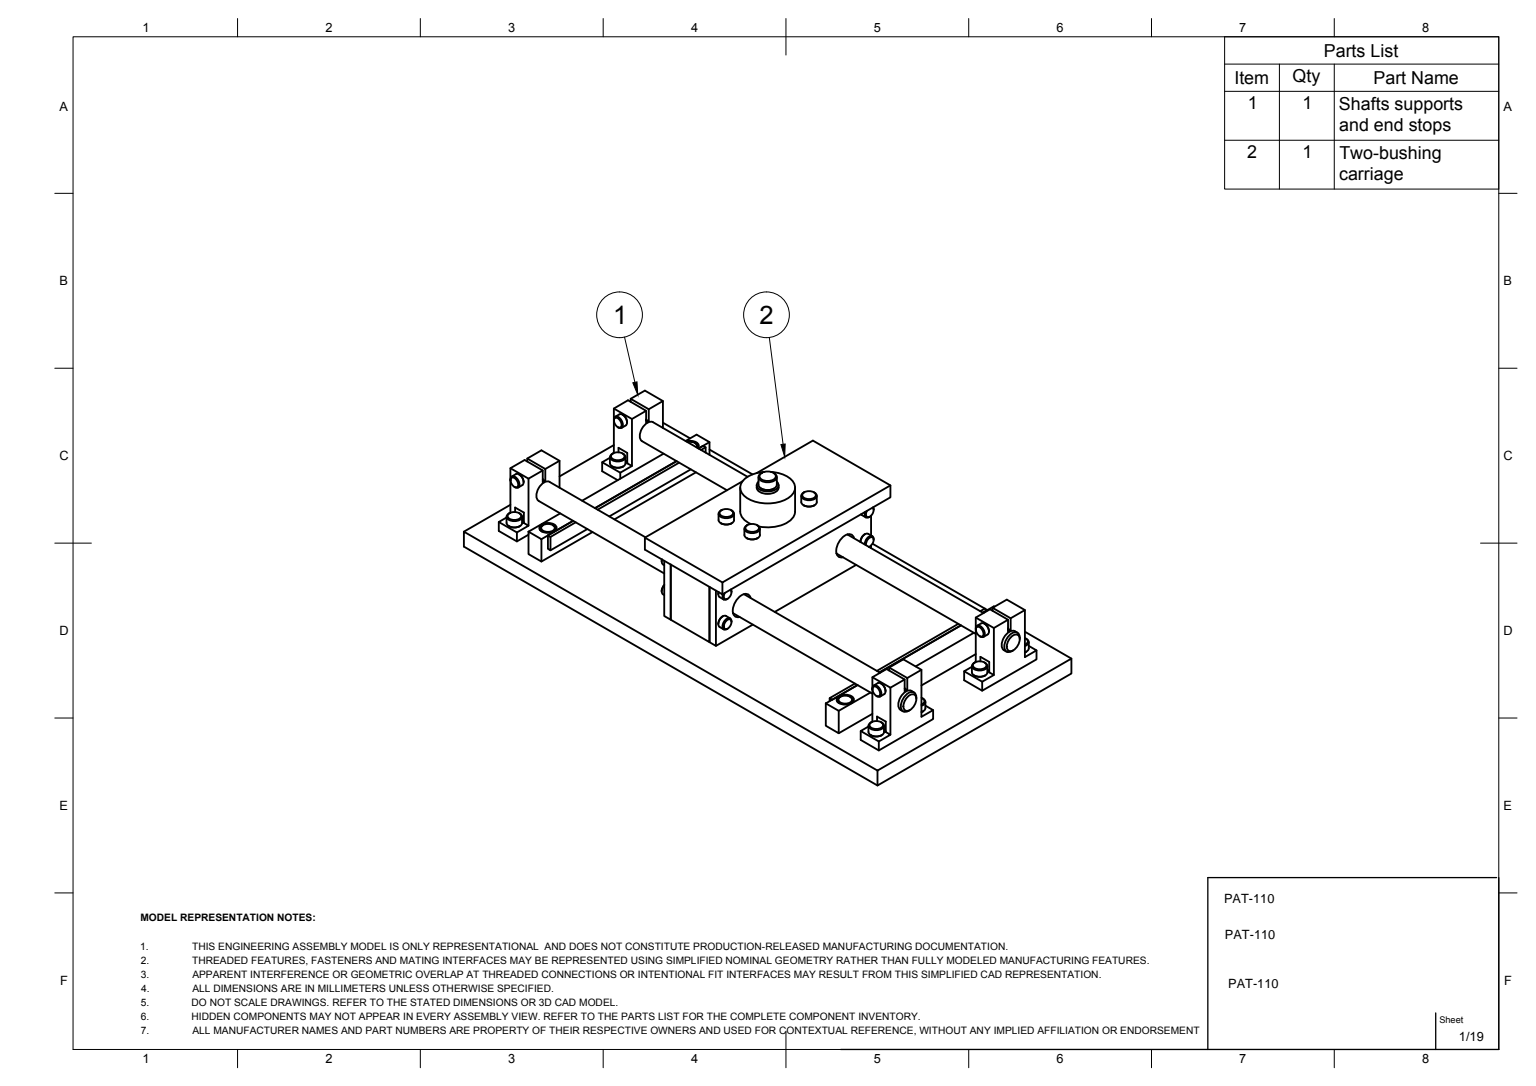
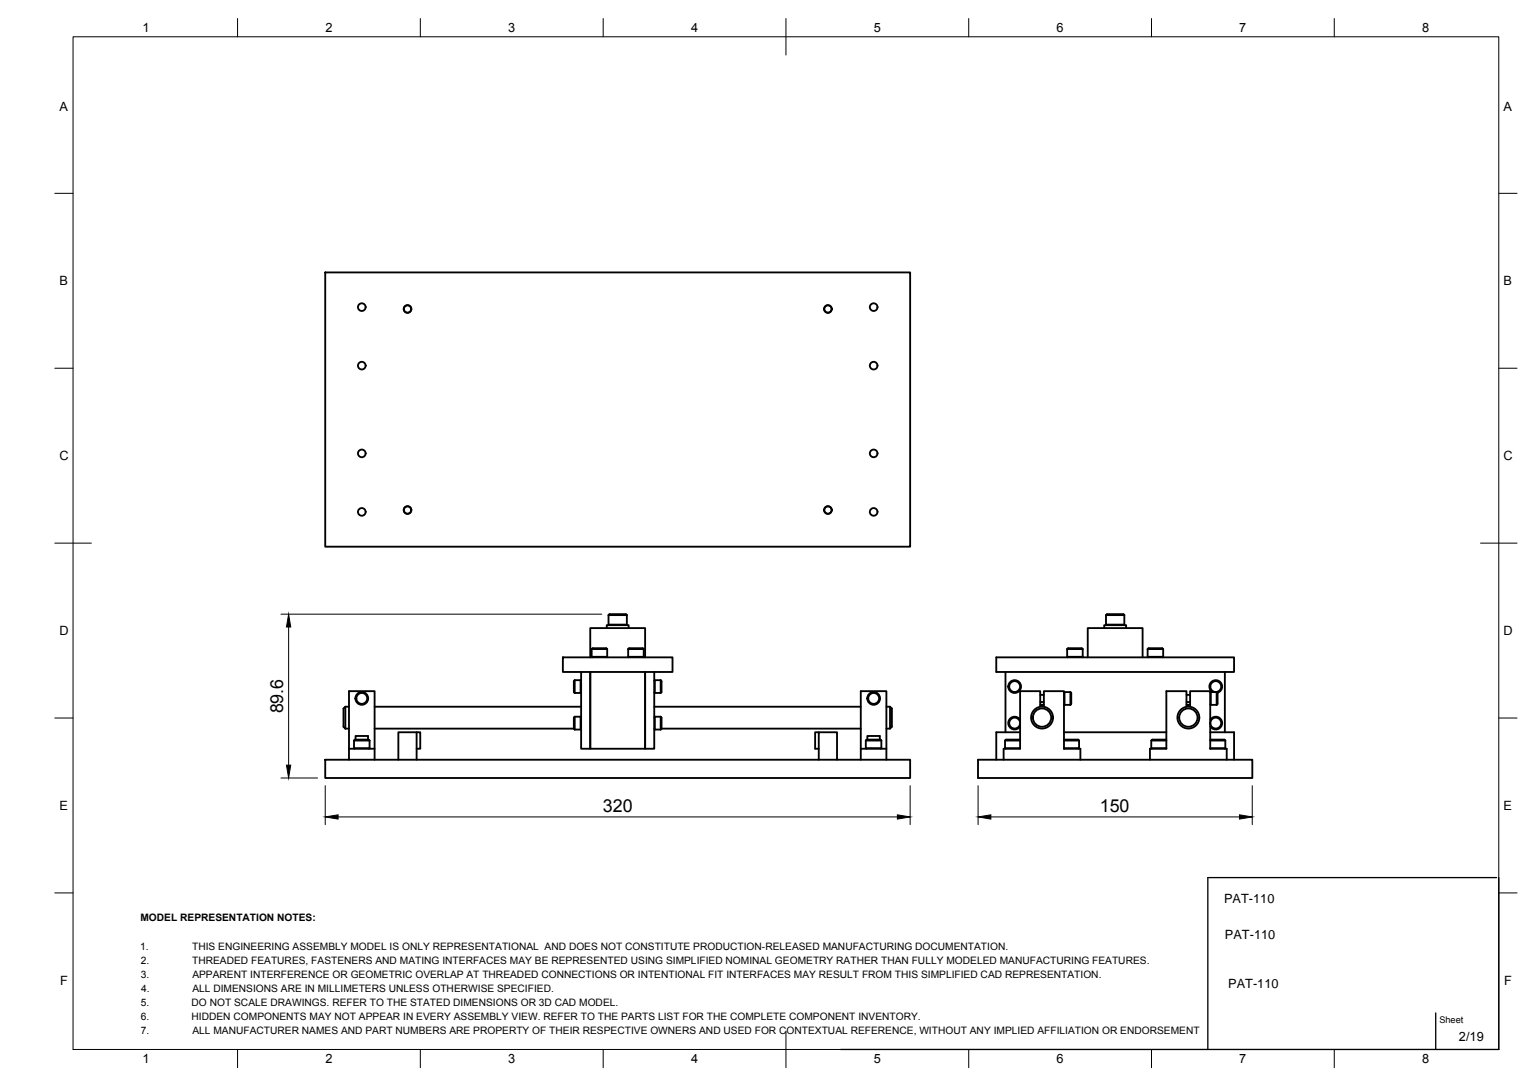
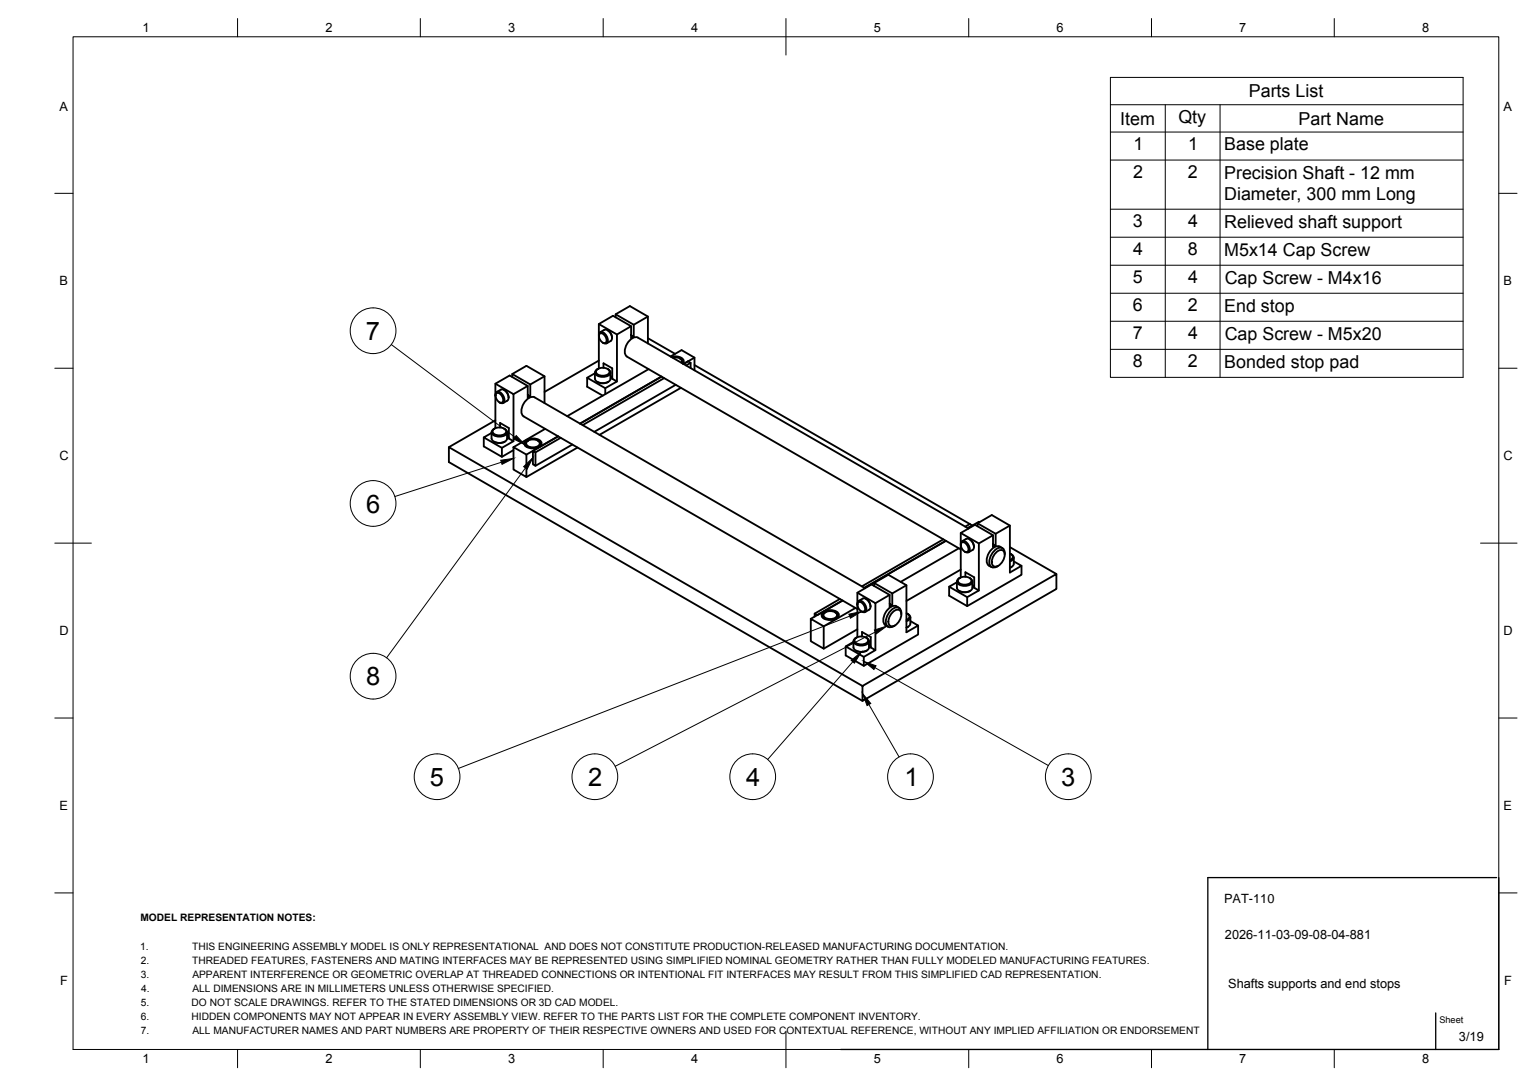
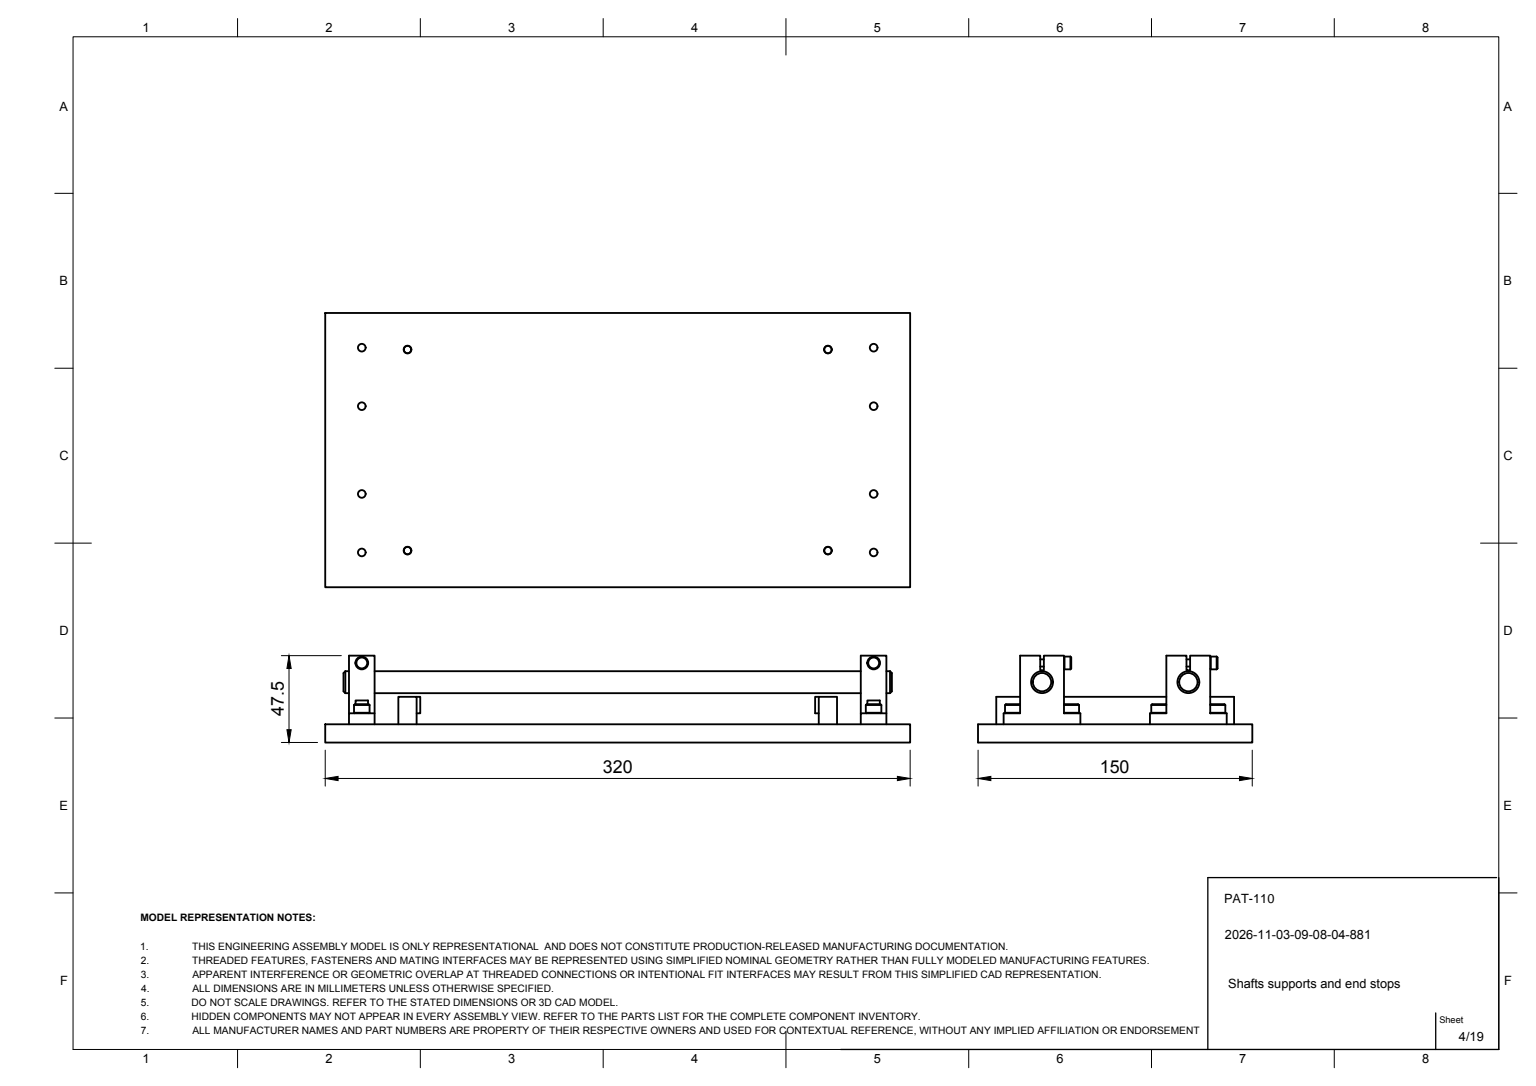
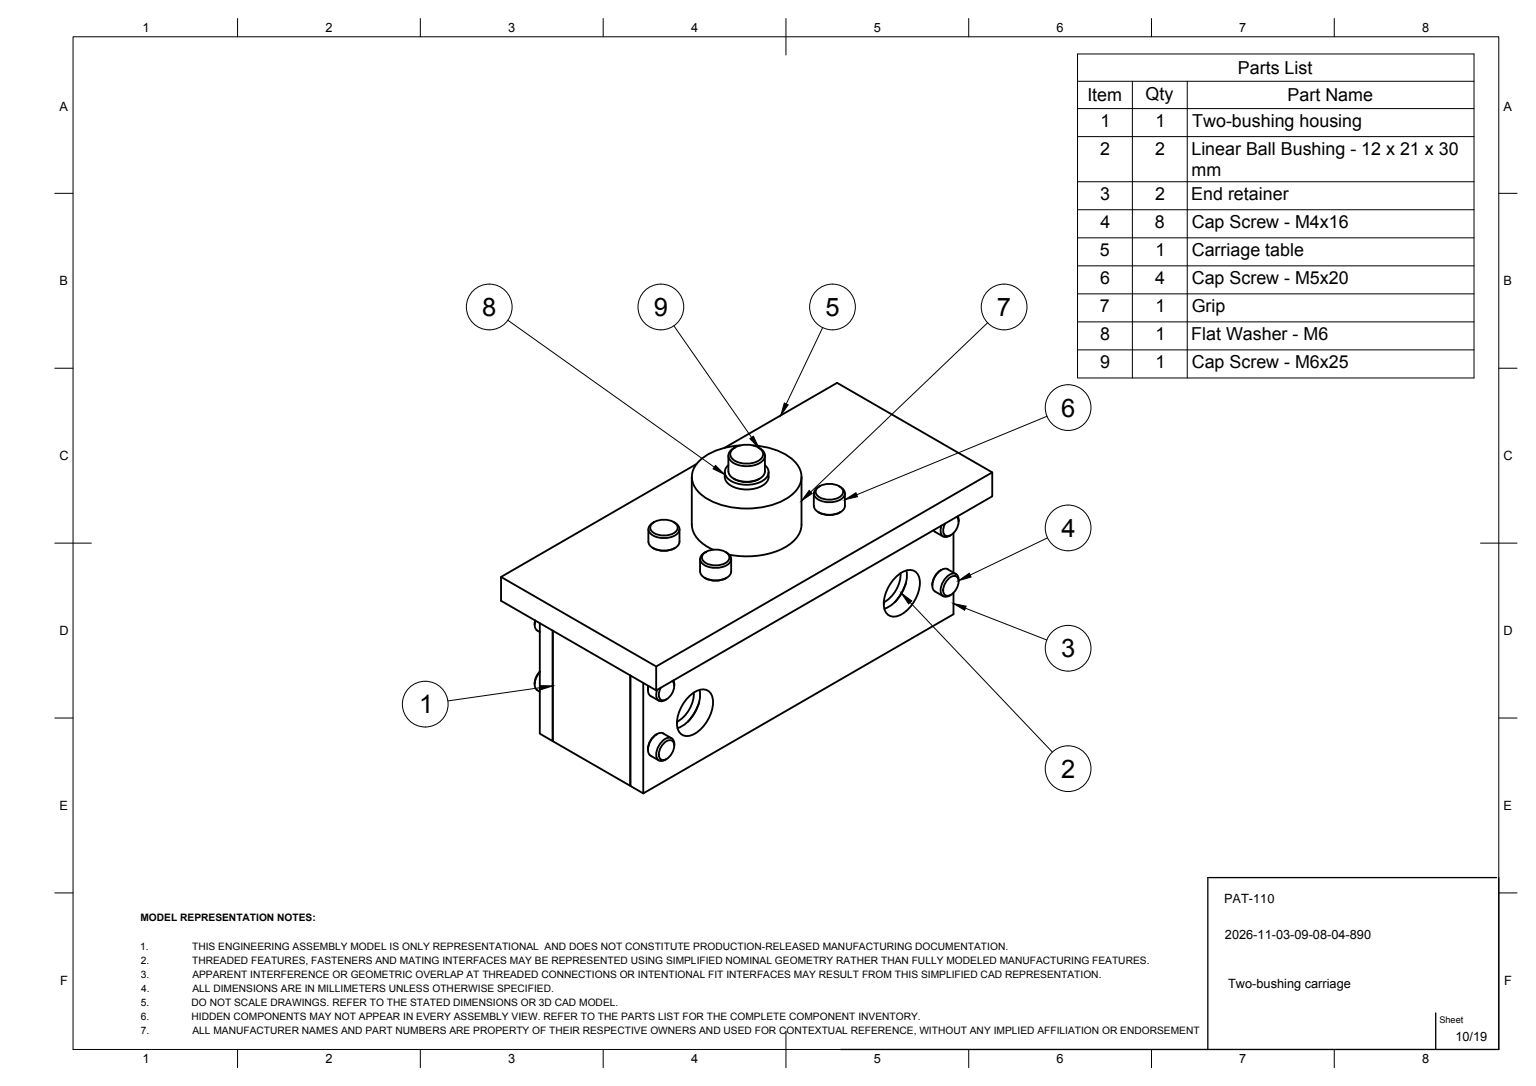
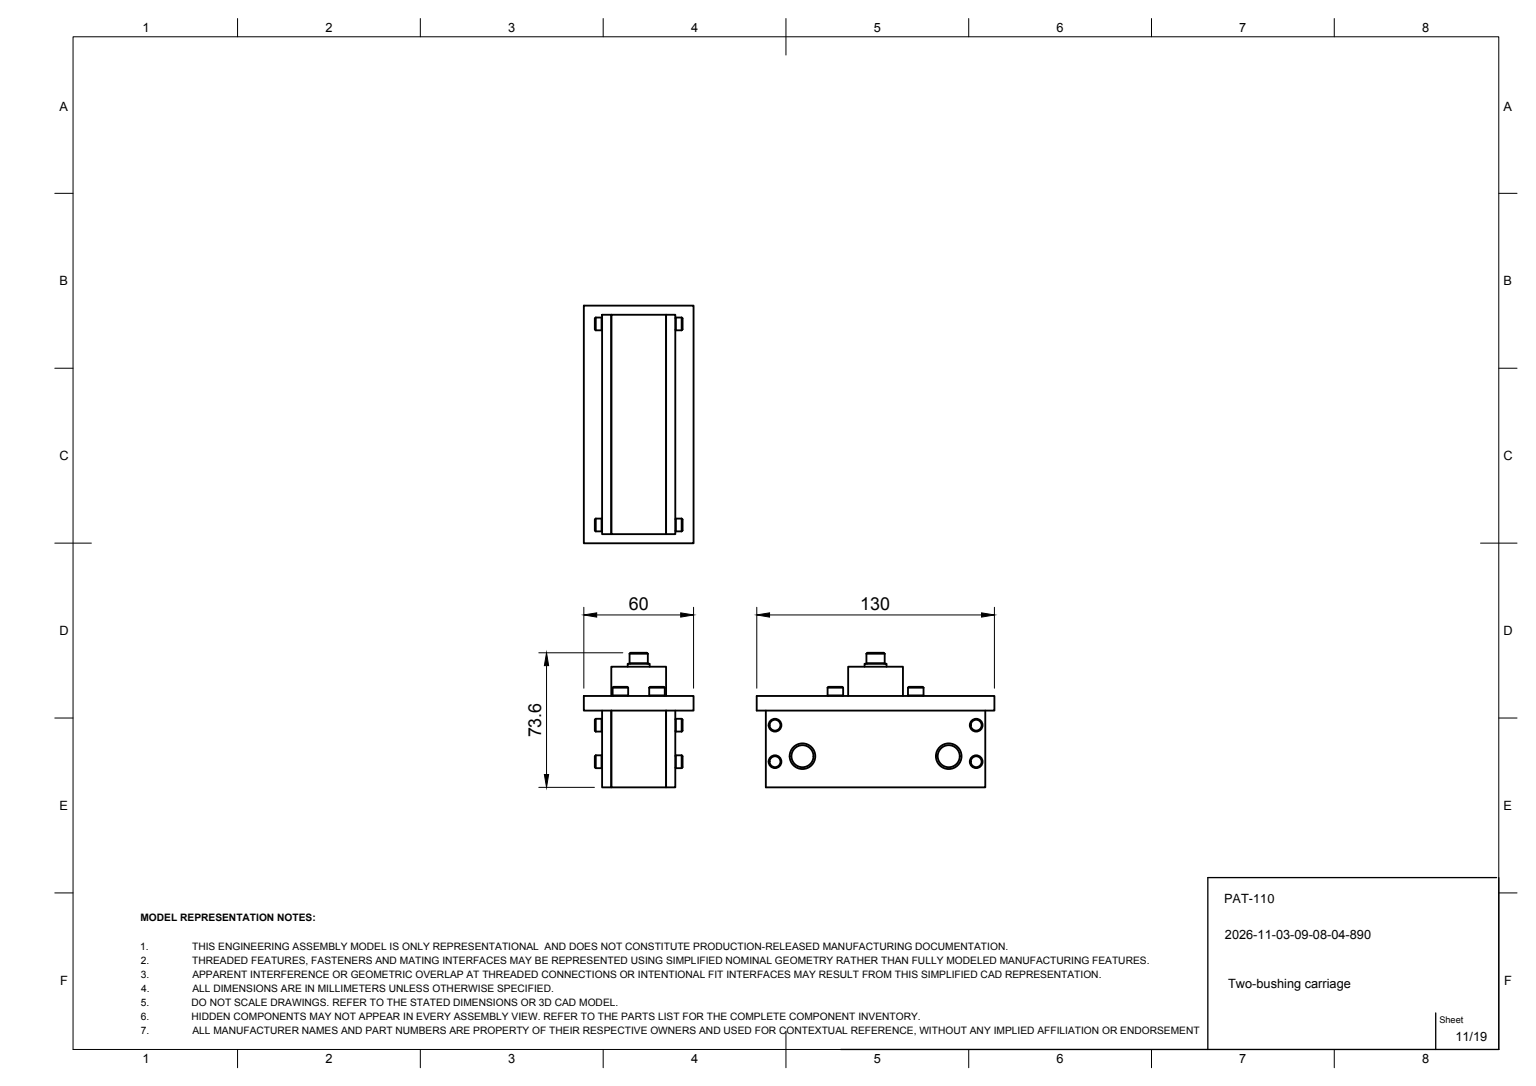
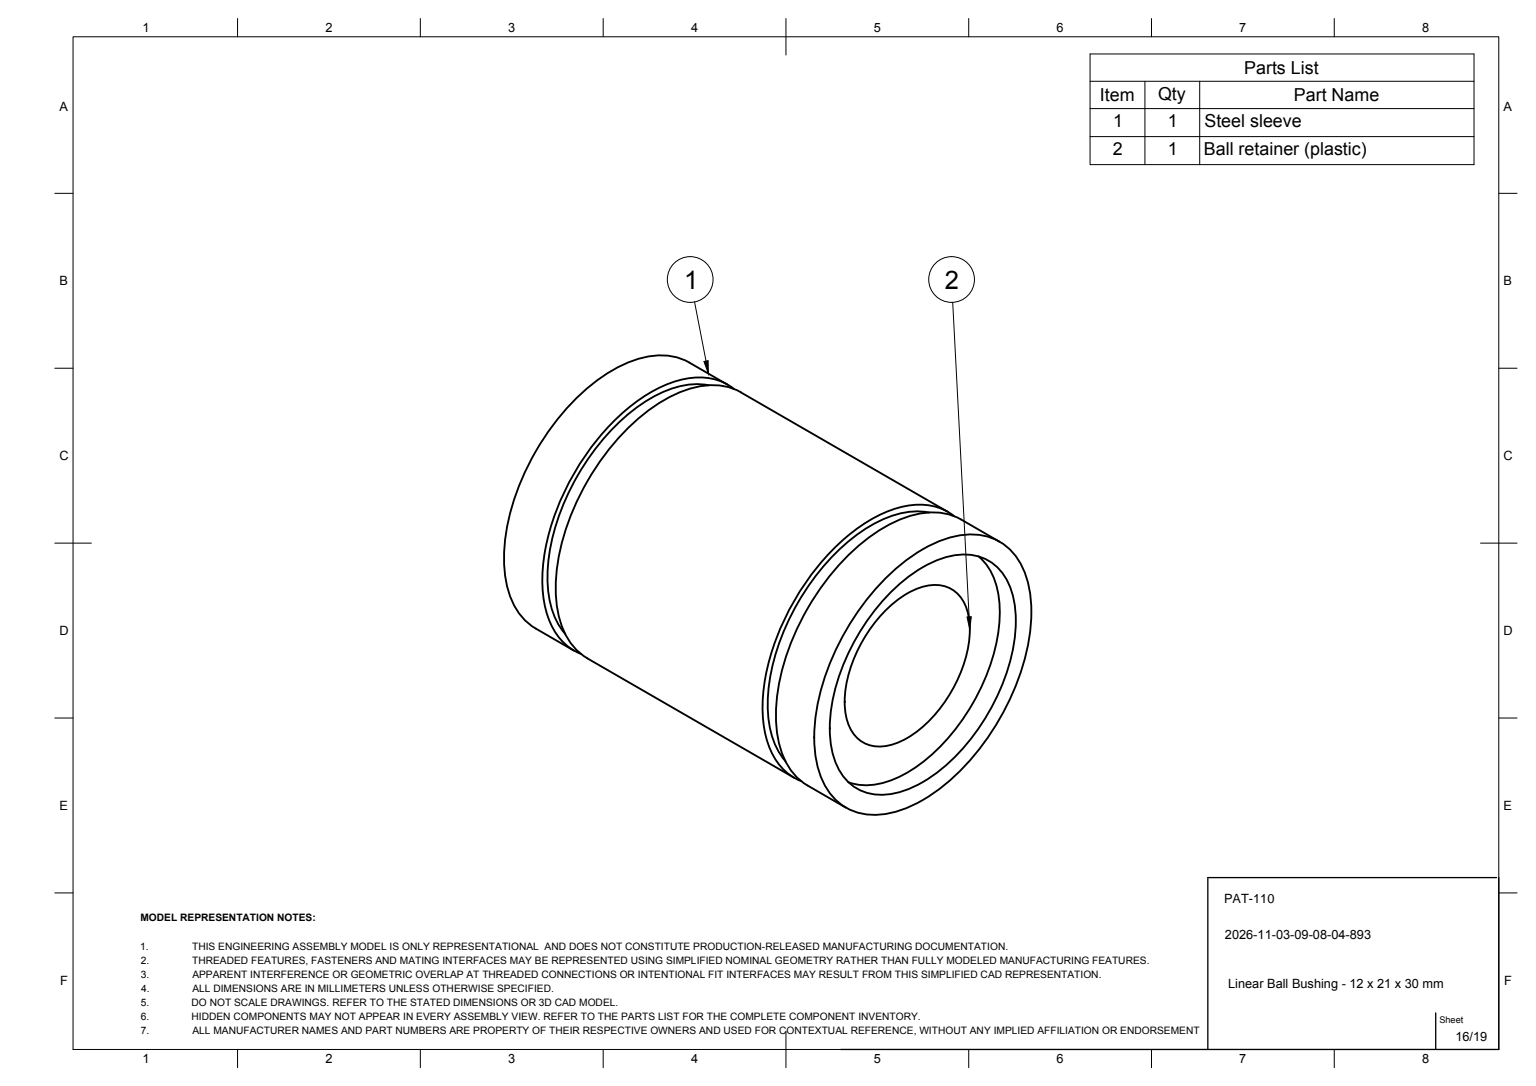
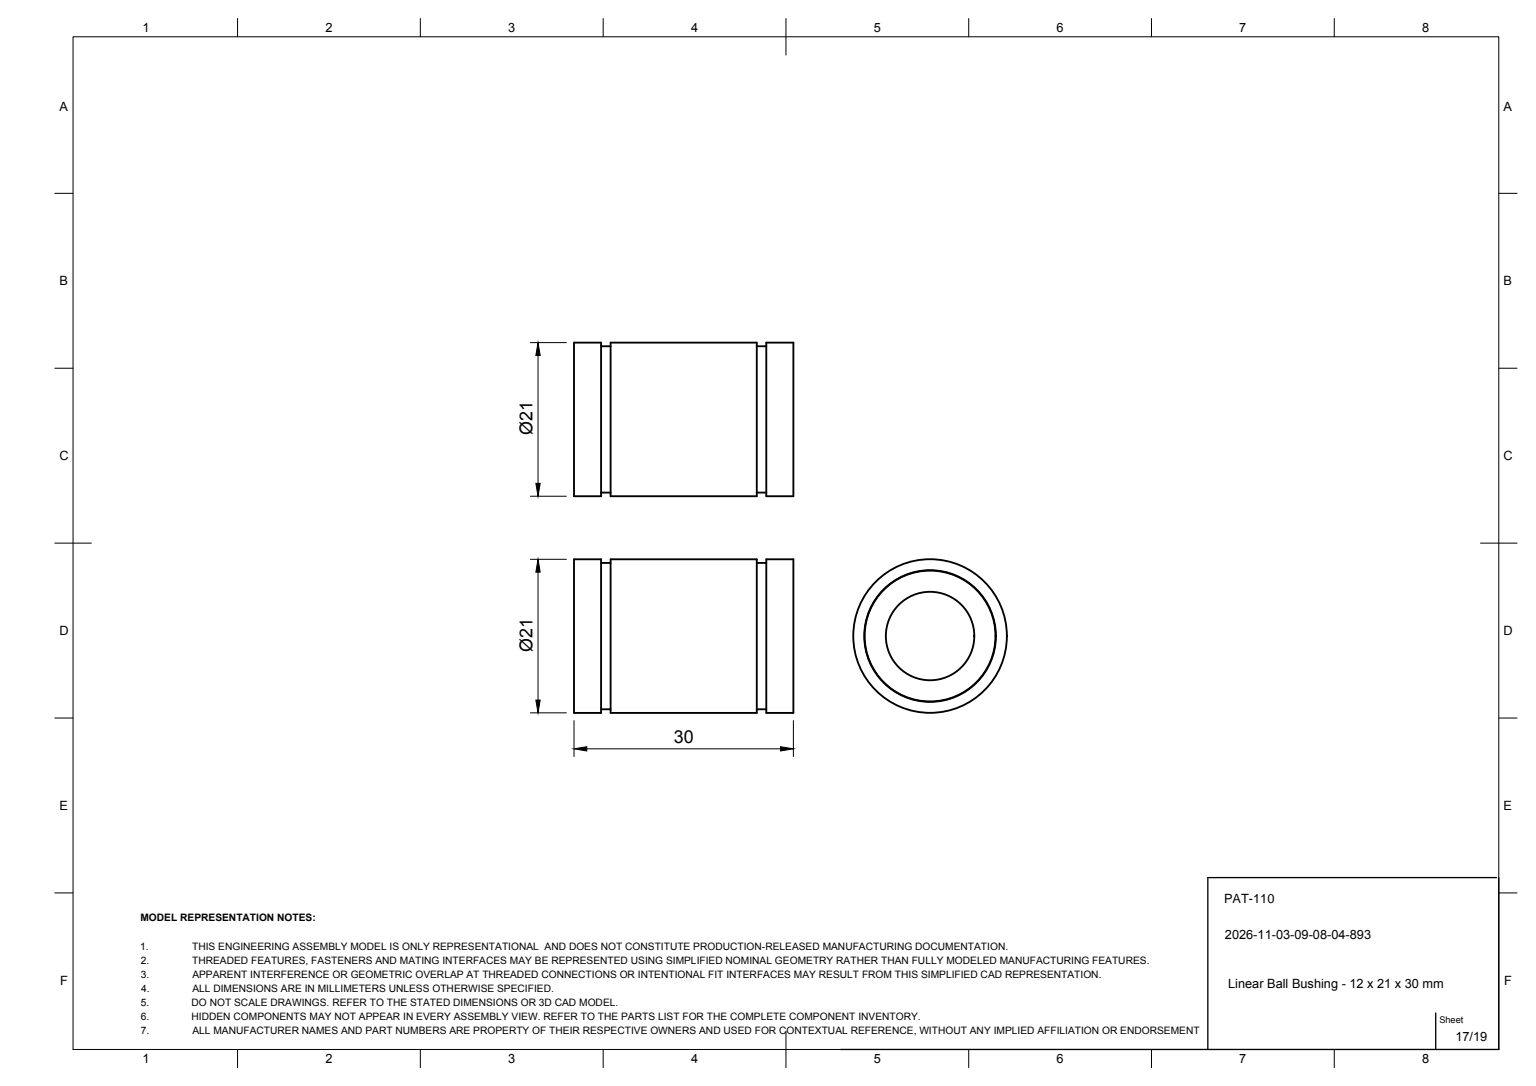
ISO-10303-21;
HEADER;
/* Generated by software containing ST-Developer
 * from STEP Tools, Inc. (www.steptools.com) 
 */

FILE_DESCRIPTION(
/* description */ ('Twin-shaft manual slide'),
/* implementation_level */ '2;1');

FILE_NAME(
/* name */ 'PAT-110',
/* time_stamp */ '2026-10-27T18:38:08-07:00',
/* author */ (''),
/* organization */ (''),
/* preprocessor_version */ 'ST-DEVELOPER v20.2',
/* originating_system */ 'Autodesk Translation Framework v15.17.0.0',
/* authorisation */ '');

FILE_SCHEMA (('AUTOMOTIVE_DESIGN { 1 0 10303 214 3 1 1 }'));
ENDSEC;

DATA;
#10=MECHANICAL_DESIGN_GEOMETRIC_PRESENTATION_REPRESENTATION('',(#276,#277,
#278,#279,#280,#281,#282,#283,#284,#285,#286,#287,#288,#289,#290,#291),
#6463);
#11=ITEM_DEFINED_TRANSFORMATION($,$,#4045,#4094);
#12=ITEM_DEFINED_TRANSFORMATION($,$,#4077,#4095);
#13=ITEM_DEFINED_TRANSFORMATION($,$,#3837,#4173);
#14=ITEM_DEFINED_TRANSFORMATION($,$,#3880,#4174);
#15=ITEM_DEFINED_TRANSFORMATION($,$,#3890,#4175);
#16=ITEM_DEFINED_TRANSFORMATION($,$,#3928,#4176);
#17=ITEM_DEFINED_TRANSFORMATION($,$,#3928,#4177);
#18=ITEM_DEFINED_TRANSFORMATION($,$,#4121,#4178);
#19=ITEM_DEFINED_TRANSFORMATION($,$,#3890,#4179);
#20=ITEM_DEFINED_TRANSFORMATION($,$,#3928,#4180);
#21=ITEM_DEFINED_TRANSFORMATION($,$,#3928,#4181);
#22=ITEM_DEFINED_TRANSFORMATION($,$,#4121,#4182);
#23=ITEM_DEFINED_TRANSFORMATION($,$,#3880,#4183);
#24=ITEM_DEFINED_TRANSFORMATION($,$,#3890,#4184);
#25=ITEM_DEFINED_TRANSFORMATION($,$,#3928,#4185);
#26=ITEM_DEFINED_TRANSFORMATION($,$,#3928,#4186);
#27=ITEM_DEFINED_TRANSFORMATION($,$,#4121,#4187);
#28=ITEM_DEFINED_TRANSFORMATION($,$,#3890,#4188);
#29=ITEM_DEFINED_TRANSFORMATION($,$,#3928,#4189);
#30=ITEM_DEFINED_TRANSFORMATION($,$,#3928,#4190);
#31=ITEM_DEFINED_TRANSFORMATION($,$,#4121,#4191);
#32=ITEM_DEFINED_TRANSFORMATION($,$,#3952,#4192);
#33=ITEM_DEFINED_TRANSFORMATION($,$,#4147,#4193);
#34=ITEM_DEFINED_TRANSFORMATION($,$,#4147,#4194);
#35=ITEM_DEFINED_TRANSFORMATION($,$,#3952,#4195);
#36=ITEM_DEFINED_TRANSFORMATION($,$,#4147,#4196);
#37=ITEM_DEFINED_TRANSFORMATION($,$,#4147,#4197);
#38=ITEM_DEFINED_TRANSFORMATION($,$,#3973,#4198);
#39=ITEM_DEFINED_TRANSFORMATION($,$,#3973,#4199);
#40=ITEM_DEFINED_TRANSFORMATION($,$,#3981,#4244);
#41=ITEM_DEFINED_TRANSFORMATION($,$,#4022,#4245);
#42=ITEM_DEFINED_TRANSFORMATION($,$,#4044,#4246);
#43=ITEM_DEFINED_TRANSFORMATION($,$,#4044,#4247);
#44=ITEM_DEFINED_TRANSFORMATION($,$,#4096,#4248);
#45=ITEM_DEFINED_TRANSFORMATION($,$,#4096,#4249);
#46=ITEM_DEFINED_TRANSFORMATION($,$,#4121,#4250);
#47=ITEM_DEFINED_TRANSFORMATION($,$,#4121,#4251);
#48=ITEM_DEFINED_TRANSFORMATION($,$,#4121,#4252);
#49=ITEM_DEFINED_TRANSFORMATION($,$,#4121,#4253);
#50=ITEM_DEFINED_TRANSFORMATION($,$,#4121,#4254);
#51=ITEM_DEFINED_TRANSFORMATION($,$,#4121,#4255);
#52=ITEM_DEFINED_TRANSFORMATION($,$,#4121,#4256);
#53=ITEM_DEFINED_TRANSFORMATION($,$,#4121,#4257);
#54=ITEM_DEFINED_TRANSFORMATION($,$,#4147,#4258);
#55=ITEM_DEFINED_TRANSFORMATION($,$,#4147,#4259);
#56=ITEM_DEFINED_TRANSFORMATION($,$,#4147,#4260);
#57=ITEM_DEFINED_TRANSFORMATION($,$,#4147,#4261);
#58=ITEM_DEFINED_TRANSFORMATION($,$,#4200,#4262);
#59=ITEM_DEFINED_TRANSFORMATION($,$,#4209,#4263);
#60=ITEM_DEFINED_TRANSFORMATION($,$,#4218,#4264);
#61=ITEM_DEFINED_TRANSFORMATION($,$,#3836,#4265);
#62=ITEM_DEFINED_TRANSFORMATION($,$,#3980,#4266);
#63=(
REPRESENTATION_RELATIONSHIP($,$,#6572,#6571)
REPRESENTATION_RELATIONSHIP_WITH_TRANSFORMATION(#11)
SHAPE_REPRESENTATION_RELATIONSHIP()
);
#64=(
REPRESENTATION_RELATIONSHIP($,$,#6573,#6571)
REPRESENTATION_RELATIONSHIP_WITH_TRANSFORMATION(#12)
SHAPE_REPRESENTATION_RELATIONSHIP()
);
#65=(
REPRESENTATION_RELATIONSHIP($,$,#6562,#6561)
REPRESENTATION_RELATIONSHIP_WITH_TRANSFORMATION(#13)
SHAPE_REPRESENTATION_RELATIONSHIP()
);
#66=(
REPRESENTATION_RELATIONSHIP($,$,#6563,#6561)
REPRESENTATION_RELATIONSHIP_WITH_TRANSFORMATION(#14)
SHAPE_REPRESENTATION_RELATIONSHIP()
);
#67=(
REPRESENTATION_RELATIONSHIP($,$,#6564,#6561)
REPRESENTATION_RELATIONSHIP_WITH_TRANSFORMATION(#15)
SHAPE_REPRESENTATION_RELATIONSHIP()
);
#68=(
REPRESENTATION_RELATIONSHIP($,$,#6565,#6561)
REPRESENTATION_RELATIONSHIP_WITH_TRANSFORMATION(#16)
SHAPE_REPRESENTATION_RELATIONSHIP()
);
#69=(
REPRESENTATION_RELATIONSHIP($,$,#6565,#6561)
REPRESENTATION_RELATIONSHIP_WITH_TRANSFORMATION(#17)
SHAPE_REPRESENTATION_RELATIONSHIP()
);
#70=(
REPRESENTATION_RELATIONSHIP($,$,#6575,#6561)
REPRESENTATION_RELATIONSHIP_WITH_TRANSFORMATION(#18)
SHAPE_REPRESENTATION_RELATIONSHIP()
);
#71=(
REPRESENTATION_RELATIONSHIP($,$,#6564,#6561)
REPRESENTATION_RELATIONSHIP_WITH_TRANSFORMATION(#19)
SHAPE_REPRESENTATION_RELATIONSHIP()
);
#72=(
REPRESENTATION_RELATIONSHIP($,$,#6565,#6561)
REPRESENTATION_RELATIONSHIP_WITH_TRANSFORMATION(#20)
SHAPE_REPRESENTATION_RELATIONSHIP()
);
#73=(
REPRESENTATION_RELATIONSHIP($,$,#6565,#6561)
REPRESENTATION_RELATIONSHIP_WITH_TRANSFORMATION(#21)
SHAPE_REPRESENTATION_RELATIONSHIP()
);
#74=(
REPRESENTATION_RELATIONSHIP($,$,#6575,#6561)
REPRESENTATION_RELATIONSHIP_WITH_TRANSFORMATION(#22)
SHAPE_REPRESENTATION_RELATIONSHIP()
);
#75=(
REPRESENTATION_RELATIONSHIP($,$,#6563,#6561)
REPRESENTATION_RELATIONSHIP_WITH_TRANSFORMATION(#23)
SHAPE_REPRESENTATION_RELATIONSHIP()
);
#76=(
REPRESENTATION_RELATIONSHIP($,$,#6564,#6561)
REPRESENTATION_RELATIONSHIP_WITH_TRANSFORMATION(#24)
SHAPE_REPRESENTATION_RELATIONSHIP()
);
#77=(
REPRESENTATION_RELATIONSHIP($,$,#6565,#6561)
REPRESENTATION_RELATIONSHIP_WITH_TRANSFORMATION(#25)
SHAPE_REPRESENTATION_RELATIONSHIP()
);
#78=(
REPRESENTATION_RELATIONSHIP($,$,#6565,#6561)
REPRESENTATION_RELATIONSHIP_WITH_TRANSFORMATION(#26)
SHAPE_REPRESENTATION_RELATIONSHIP()
);
#79=(
REPRESENTATION_RELATIONSHIP($,$,#6575,#6561)
REPRESENTATION_RELATIONSHIP_WITH_TRANSFORMATION(#27)
SHAPE_REPRESENTATION_RELATIONSHIP()
);
#80=(
REPRESENTATION_RELATIONSHIP($,$,#6564,#6561)
REPRESENTATION_RELATIONSHIP_WITH_TRANSFORMATION(#28)
SHAPE_REPRESENTATION_RELATIONSHIP()
);
#81=(
REPRESENTATION_RELATIONSHIP($,$,#6565,#6561)
REPRESENTATION_RELATIONSHIP_WITH_TRANSFORMATION(#29)
SHAPE_REPRESENTATION_RELATIONSHIP()
);
#82=(
REPRESENTATION_RELATIONSHIP($,$,#6565,#6561)
REPRESENTATION_RELATIONSHIP_WITH_TRANSFORMATION(#30)
SHAPE_REPRESENTATION_RELATIONSHIP()
);
#83=(
REPRESENTATION_RELATIONSHIP($,$,#6575,#6561)
REPRESENTATION_RELATIONSHIP_WITH_TRANSFORMATION(#31)
SHAPE_REPRESENTATION_RELATIONSHIP()
);
#84=(
REPRESENTATION_RELATIONSHIP($,$,#6566,#6561)
REPRESENTATION_RELATIONSHIP_WITH_TRANSFORMATION(#32)
SHAPE_REPRESENTATION_RELATIONSHIP()
);
#85=(
REPRESENTATION_RELATIONSHIP($,$,#6576,#6561)
REPRESENTATION_RELATIONSHIP_WITH_TRANSFORMATION(#33)
SHAPE_REPRESENTATION_RELATIONSHIP()
);
#86=(
REPRESENTATION_RELATIONSHIP($,$,#6576,#6561)
REPRESENTATION_RELATIONSHIP_WITH_TRANSFORMATION(#34)
SHAPE_REPRESENTATION_RELATIONSHIP()
);
#87=(
REPRESENTATION_RELATIONSHIP($,$,#6566,#6561)
REPRESENTATION_RELATIONSHIP_WITH_TRANSFORMATION(#35)
SHAPE_REPRESENTATION_RELATIONSHIP()
);
#88=(
REPRESENTATION_RELATIONSHIP($,$,#6576,#6561)
REPRESENTATION_RELATIONSHIP_WITH_TRANSFORMATION(#36)
SHAPE_REPRESENTATION_RELATIONSHIP()
);
#89=(
REPRESENTATION_RELATIONSHIP($,$,#6576,#6561)
REPRESENTATION_RELATIONSHIP_WITH_TRANSFORMATION(#37)
SHAPE_REPRESENTATION_RELATIONSHIP()
);
#90=(
REPRESENTATION_RELATIONSHIP($,$,#6567,#6561)
REPRESENTATION_RELATIONSHIP_WITH_TRANSFORMATION(#38)
SHAPE_REPRESENTATION_RELATIONSHIP()
);
#91=(
REPRESENTATION_RELATIONSHIP($,$,#6567,#6561)
REPRESENTATION_RELATIONSHIP_WITH_TRANSFORMATION(#39)
SHAPE_REPRESENTATION_RELATIONSHIP()
);
#92=(
REPRESENTATION_RELATIONSHIP($,$,#6569,#6568)
REPRESENTATION_RELATIONSHIP_WITH_TRANSFORMATION(#40)
SHAPE_REPRESENTATION_RELATIONSHIP()
);
#93=(
REPRESENTATION_RELATIONSHIP($,$,#6570,#6568)
REPRESENTATION_RELATIONSHIP_WITH_TRANSFORMATION(#41)
SHAPE_REPRESENTATION_RELATIONSHIP()
);
#94=(
REPRESENTATION_RELATIONSHIP($,$,#6571,#6568)
REPRESENTATION_RELATIONSHIP_WITH_TRANSFORMATION(#42)
SHAPE_REPRESENTATION_RELATIONSHIP()
);
#95=(
REPRESENTATION_RELATIONSHIP($,$,#6571,#6568)
REPRESENTATION_RELATIONSHIP_WITH_TRANSFORMATION(#43)
SHAPE_REPRESENTATION_RELATIONSHIP()
);
#96=(
REPRESENTATION_RELATIONSHIP($,$,#6574,#6568)
REPRESENTATION_RELATIONSHIP_WITH_TRANSFORMATION(#44)
SHAPE_REPRESENTATION_RELATIONSHIP()
);
#97=(
REPRESENTATION_RELATIONSHIP($,$,#6574,#6568)
REPRESENTATION_RELATIONSHIP_WITH_TRANSFORMATION(#45)
SHAPE_REPRESENTATION_RELATIONSHIP()
);
#98=(
REPRESENTATION_RELATIONSHIP($,$,#6575,#6568)
REPRESENTATION_RELATIONSHIP_WITH_TRANSFORMATION(#46)
SHAPE_REPRESENTATION_RELATIONSHIP()
);
#99=(
REPRESENTATION_RELATIONSHIP($,$,#6575,#6568)
REPRESENTATION_RELATIONSHIP_WITH_TRANSFORMATION(#47)
SHAPE_REPRESENTATION_RELATIONSHIP()
);
#100=(
REPRESENTATION_RELATIONSHIP($,$,#6575,#6568)
REPRESENTATION_RELATIONSHIP_WITH_TRANSFORMATION(#48)
SHAPE_REPRESENTATION_RELATIONSHIP()
);
#101=(
REPRESENTATION_RELATIONSHIP($,$,#6575,#6568)
REPRESENTATION_RELATIONSHIP_WITH_TRANSFORMATION(#49)
SHAPE_REPRESENTATION_RELATIONSHIP()
);
#102=(
REPRESENTATION_RELATIONSHIP($,$,#6575,#6568)
REPRESENTATION_RELATIONSHIP_WITH_TRANSFORMATION(#50)
SHAPE_REPRESENTATION_RELATIONSHIP()
);
#103=(
REPRESENTATION_RELATIONSHIP($,$,#6575,#6568)
REPRESENTATION_RELATIONSHIP_WITH_TRANSFORMATION(#51)
SHAPE_REPRESENTATION_RELATIONSHIP()
);
#104=(
REPRESENTATION_RELATIONSHIP($,$,#6575,#6568)
REPRESENTATION_RELATIONSHIP_WITH_TRANSFORMATION(#52)
SHAPE_REPRESENTATION_RELATIONSHIP()
);
#105=(
REPRESENTATION_RELATIONSHIP($,$,#6575,#6568)
REPRESENTATION_RELATIONSHIP_WITH_TRANSFORMATION(#53)
SHAPE_REPRESENTATION_RELATIONSHIP()
);
#106=(
REPRESENTATION_RELATIONSHIP($,$,#6576,#6568)
REPRESENTATION_RELATIONSHIP_WITH_TRANSFORMATION(#54)
SHAPE_REPRESENTATION_RELATIONSHIP()
);
#107=(
REPRESENTATION_RELATIONSHIP($,$,#6576,#6568)
REPRESENTATION_RELATIONSHIP_WITH_TRANSFORMATION(#55)
SHAPE_REPRESENTATION_RELATIONSHIP()
);
#108=(
REPRESENTATION_RELATIONSHIP($,$,#6576,#6568)
REPRESENTATION_RELATIONSHIP_WITH_TRANSFORMATION(#56)
SHAPE_REPRESENTATION_RELATIONSHIP()
);
#109=(
REPRESENTATION_RELATIONSHIP($,$,#6576,#6568)
REPRESENTATION_RELATIONSHIP_WITH_TRANSFORMATION(#57)
SHAPE_REPRESENTATION_RELATIONSHIP()
);
#110=(
REPRESENTATION_RELATIONSHIP($,$,#6577,#6568)
REPRESENTATION_RELATIONSHIP_WITH_TRANSFORMATION(#58)
SHAPE_REPRESENTATION_RELATIONSHIP()
);
#111=(
REPRESENTATION_RELATIONSHIP($,$,#6578,#6568)
REPRESENTATION_RELATIONSHIP_WITH_TRANSFORMATION(#59)
SHAPE_REPRESENTATION_RELATIONSHIP()
);
#112=(
REPRESENTATION_RELATIONSHIP($,$,#6579,#6568)
REPRESENTATION_RELATIONSHIP_WITH_TRANSFORMATION(#60)
SHAPE_REPRESENTATION_RELATIONSHIP()
);
#113=(
REPRESENTATION_RELATIONSHIP($,$,#6561,#6560)
REPRESENTATION_RELATIONSHIP_WITH_TRANSFORMATION(#61)
SHAPE_REPRESENTATION_RELATIONSHIP()
);
#114=(
REPRESENTATION_RELATIONSHIP($,$,#6568,#6560)
REPRESENTATION_RELATIONSHIP_WITH_TRANSFORMATION(#62)
SHAPE_REPRESENTATION_RELATIONSHIP()
);
#115=CONTEXT_DEPENDENT_SHAPE_REPRESENTATION(#63,#6502);
#116=CONTEXT_DEPENDENT_SHAPE_REPRESENTATION(#64,#6503);
#117=CONTEXT_DEPENDENT_SHAPE_REPRESENTATION(#65,#6507);
#118=CONTEXT_DEPENDENT_SHAPE_REPRESENTATION(#66,#6508);
#119=CONTEXT_DEPENDENT_SHAPE_REPRESENTATION(#67,#6509);
#120=CONTEXT_DEPENDENT_SHAPE_REPRESENTATION(#68,#6510);
#121=CONTEXT_DEPENDENT_SHAPE_REPRESENTATION(#69,#6511);
#122=CONTEXT_DEPENDENT_SHAPE_REPRESENTATION(#70,#6512);
#123=CONTEXT_DEPENDENT_SHAPE_REPRESENTATION(#71,#6513);
#124=CONTEXT_DEPENDENT_SHAPE_REPRESENTATION(#72,#6514);
#125=CONTEXT_DEPENDENT_SHAPE_REPRESENTATION(#73,#6515);
#126=CONTEXT_DEPENDENT_SHAPE_REPRESENTATION(#74,#6516);
#127=CONTEXT_DEPENDENT_SHAPE_REPRESENTATION(#75,#6517);
#128=CONTEXT_DEPENDENT_SHAPE_REPRESENTATION(#76,#6518);
#129=CONTEXT_DEPENDENT_SHAPE_REPRESENTATION(#77,#6519);
#130=CONTEXT_DEPENDENT_SHAPE_REPRESENTATION(#78,#6520);
#131=CONTEXT_DEPENDENT_SHAPE_REPRESENTATION(#79,#6521);
#132=CONTEXT_DEPENDENT_SHAPE_REPRESENTATION(#80,#6522);
#133=CONTEXT_DEPENDENT_SHAPE_REPRESENTATION(#81,#6523);
#134=CONTEXT_DEPENDENT_SHAPE_REPRESENTATION(#82,#6524);
#135=CONTEXT_DEPENDENT_SHAPE_REPRESENTATION(#83,#6525);
#136=CONTEXT_DEPENDENT_SHAPE_REPRESENTATION(#84,#6526);
#137=CONTEXT_DEPENDENT_SHAPE_REPRESENTATION(#85,#6527);
#138=CONTEXT_DEPENDENT_SHAPE_REPRESENTATION(#86,#6528);
#139=CONTEXT_DEPENDENT_SHAPE_REPRESENTATION(#87,#6529);
#140=CONTEXT_DEPENDENT_SHAPE_REPRESENTATION(#88,#6530);
#141=CONTEXT_DEPENDENT_SHAPE_REPRESENTATION(#89,#6531);
#142=CONTEXT_DEPENDENT_SHAPE_REPRESENTATION(#90,#6532);
#143=CONTEXT_DEPENDENT_SHAPE_REPRESENTATION(#91,#6533);
#144=CONTEXT_DEPENDENT_SHAPE_REPRESENTATION(#92,#6537);
#145=CONTEXT_DEPENDENT_SHAPE_REPRESENTATION(#93,#6538);
#146=CONTEXT_DEPENDENT_SHAPE_REPRESENTATION(#94,#6539);
#147=CONTEXT_DEPENDENT_SHAPE_REPRESENTATION(#95,#6540);
#148=CONTEXT_DEPENDENT_SHAPE_REPRESENTATION(#96,#6541);
#149=CONTEXT_DEPENDENT_SHAPE_REPRESENTATION(#97,#6542);
#150=CONTEXT_DEPENDENT_SHAPE_REPRESENTATION(#98,#6543);
#151=CONTEXT_DEPENDENT_SHAPE_REPRESENTATION(#99,#6544);
#152=CONTEXT_DEPENDENT_SHAPE_REPRESENTATION(#100,#6545);
#153=CONTEXT_DEPENDENT_SHAPE_REPRESENTATION(#101,#6546);
#154=CONTEXT_DEPENDENT_SHAPE_REPRESENTATION(#102,#6547);
#155=CONTEXT_DEPENDENT_SHAPE_REPRESENTATION(#103,#6548);
#156=CONTEXT_DEPENDENT_SHAPE_REPRESENTATION(#104,#6549);
#157=CONTEXT_DEPENDENT_SHAPE_REPRESENTATION(#105,#6550);
#158=CONTEXT_DEPENDENT_SHAPE_REPRESENTATION(#106,#6551);
#159=CONTEXT_DEPENDENT_SHAPE_REPRESENTATION(#107,#6552);
#160=CONTEXT_DEPENDENT_SHAPE_REPRESENTATION(#108,#6553);
#161=CONTEXT_DEPENDENT_SHAPE_REPRESENTATION(#109,#6554);
#162=CONTEXT_DEPENDENT_SHAPE_REPRESENTATION(#110,#6555);
#163=CONTEXT_DEPENDENT_SHAPE_REPRESENTATION(#111,#6556);
#164=CONTEXT_DEPENDENT_SHAPE_REPRESENTATION(#112,#6557);
#165=CONTEXT_DEPENDENT_SHAPE_REPRESENTATION(#113,#6558);
#166=CONTEXT_DEPENDENT_SHAPE_REPRESENTATION(#114,#6559);
#167=NEXT_ASSEMBLY_USAGE_OCCURRENCE('Steel sleeve:1','Steel sleeve:1',
'Steel sleeve:1',#6592,#6593,'Steel sleeve:1');
#168=NEXT_ASSEMBLY_USAGE_OCCURRENCE('Ball retainer (plastic):1',
'Ball retainer (plastic):1','Ball retainer (plastic):1',#6592,#6594,
'Ball retainer (plastic):1');
#169=NEXT_ASSEMBLY_USAGE_OCCURRENCE('Base plate:2','Base plate:2',
'Base plate:2',#6582,#6583,'Base plate:2');
#170=NEXT_ASSEMBLY_USAGE_OCCURRENCE(
'Precision Shaft - 12 mm Diameter, 300 mm Long:2',
'Precision Shaft - 12 mm Diameter, 300 mm Long:2',
'Precision Shaft - 12 mm Diameter, 300 mm Long:2',#6582,#6584,
'Precision Shaft - 12 mm Diameter, 300 mm Long:2');
#171=NEXT_ASSEMBLY_USAGE_OCCURRENCE('Relieved shaft support:2',
'Relieved shaft support:2','Relieved shaft support:2',#6582,#6585,
'Relieved shaft support:2');
#172=NEXT_ASSEMBLY_USAGE_OCCURRENCE('M5x14 Cap Screw:2',
'M5x14 Cap Screw:2','M5x14 Cap Screw:2',#6582,#6586,'M5x14 Cap Screw:2');
#173=NEXT_ASSEMBLY_USAGE_OCCURRENCE('M5x14 Cap Screw:3',
'M5x14 Cap Screw:3','M5x14 Cap Screw:3',#6582,#6586,'M5x14 Cap Screw:3');
#174=NEXT_ASSEMBLY_USAGE_OCCURRENCE('Cap Screw - M4x16:2',
'Cap Screw - M4x16:2','Cap Screw - M4x16:2',#6582,#6596,
'Cap Screw - M4x16:2');
#175=NEXT_ASSEMBLY_USAGE_OCCURRENCE('Relieved shaft support:3',
'Relieved shaft support:3','Relieved shaft support:3',#6582,#6585,
'Relieved shaft support:3');
#176=NEXT_ASSEMBLY_USAGE_OCCURRENCE('M5x14 Cap Screw:4',
'M5x14 Cap Screw:4','M5x14 Cap Screw:4',#6582,#6586,'M5x14 Cap Screw:4');
#177=NEXT_ASSEMBLY_USAGE_OCCURRENCE('M5x14 Cap Screw:5',
'M5x14 Cap Screw:5','M5x14 Cap Screw:5',#6582,#6586,'M5x14 Cap Screw:5');
#178=NEXT_ASSEMBLY_USAGE_OCCURRENCE('Cap Screw - M4x16:3',
'Cap Screw - M4x16:3','Cap Screw - M4x16:3',#6582,#6596,
'Cap Screw - M4x16:3');
#179=NEXT_ASSEMBLY_USAGE_OCCURRENCE(
'Precision Shaft - 12 mm Diameter, 300 mm Long:3',
'Precision Shaft - 12 mm Diameter, 300 mm Long:3',
'Precision Shaft - 12 mm Diameter, 300 mm Long:3',#6582,#6584,
'Precision Shaft - 12 mm Diameter, 300 mm Long:3');
#180=NEXT_ASSEMBLY_USAGE_OCCURRENCE('Relieved shaft support:4',
'Relieved shaft support:4','Relieved shaft support:4',#6582,#6585,
'Relieved shaft support:4');
#181=NEXT_ASSEMBLY_USAGE_OCCURRENCE('M5x14 Cap Screw:6',
'M5x14 Cap Screw:6','M5x14 Cap Screw:6',#6582,#6586,'M5x14 Cap Screw:6');
#182=NEXT_ASSEMBLY_USAGE_OCCURRENCE('M5x14 Cap Screw:7',
'M5x14 Cap Screw:7','M5x14 Cap Screw:7',#6582,#6586,'M5x14 Cap Screw:7');
#183=NEXT_ASSEMBLY_USAGE_OCCURRENCE('Cap Screw - M4x16:4',
'Cap Screw - M4x16:4','Cap Screw - M4x16:4',#6582,#6596,
'Cap Screw - M4x16:4');
#184=NEXT_ASSEMBLY_USAGE_OCCURRENCE('Relieved shaft support:5',
'Relieved shaft support:5','Relieved shaft support:5',#6582,#6585,
'Relieved shaft support:5');
#185=NEXT_ASSEMBLY_USAGE_OCCURRENCE('M5x14 Cap Screw:8',
'M5x14 Cap Screw:8','M5x14 Cap Screw:8',#6582,#6586,'M5x14 Cap Screw:8');
#186=NEXT_ASSEMBLY_USAGE_OCCURRENCE('M5x14 Cap Screw:9',
'M5x14 Cap Screw:9','M5x14 Cap Screw:9',#6582,#6586,'M5x14 Cap Screw:9');
#187=NEXT_ASSEMBLY_USAGE_OCCURRENCE('Cap Screw - M4x16:5',
'Cap Screw - M4x16:5','Cap Screw - M4x16:5',#6582,#6596,
'Cap Screw - M4x16:5');
#188=NEXT_ASSEMBLY_USAGE_OCCURRENCE('End stop:2','End stop:2',
'End stop:2',#6582,#6587,'End stop:2');
#189=NEXT_ASSEMBLY_USAGE_OCCURRENCE('Cap Screw - M5x20:6',
'Cap Screw - M5x20:6','Cap Screw - M5x20:6',#6582,#6597,
'Cap Screw - M5x20:6');
#190=NEXT_ASSEMBLY_USAGE_OCCURRENCE('Cap Screw - M5x20:7',
'Cap Screw - M5x20:7','Cap Screw - M5x20:7',#6582,#6597,
'Cap Screw - M5x20:7');
#191=NEXT_ASSEMBLY_USAGE_OCCURRENCE('End stop:3','End stop:3',
'End stop:3',#6582,#6587,'End stop:3');
#192=NEXT_ASSEMBLY_USAGE_OCCURRENCE('Cap Screw - M5x20:8',
'Cap Screw - M5x20:8','Cap Screw - M5x20:8',#6582,#6597,
'Cap Screw - M5x20:8');
#193=NEXT_ASSEMBLY_USAGE_OCCURRENCE('Cap Screw - M5x20:9',
'Cap Screw - M5x20:9','Cap Screw - M5x20:9',#6582,#6597,
'Cap Screw - M5x20:9');
#194=NEXT_ASSEMBLY_USAGE_OCCURRENCE('Bonded stop pad:2',
'Bonded stop pad:2','Bonded stop pad:2',#6582,#6588,'Bonded stop pad:2');
#195=NEXT_ASSEMBLY_USAGE_OCCURRENCE('Bonded stop pad:3',
'Bonded stop pad:3','Bonded stop pad:3',#6582,#6588,'Bonded stop pad:3');
#196=NEXT_ASSEMBLY_USAGE_OCCURRENCE('Two-bushing housing:1',
'Two-bushing housing:1','Two-bushing housing:1',#6589,#6590,
'Two-bushing housing:1');
#197=NEXT_ASSEMBLY_USAGE_OCCURRENCE('Carriage table:1',
'Carriage table:1','Carriage table:1',#6589,#6591,'Carriage table:1');
#198=NEXT_ASSEMBLY_USAGE_OCCURRENCE(
'Linear Ball Bushing - 12 x 21 x 30 mm:2',
'Linear Ball Bushing - 12 x 21 x 30 mm:2',
'Linear Ball Bushing - 12 x 21 x 30 mm:2',#6589,#6592,
'Linear Ball Bushing - 12 x 21 x 30 mm:2');
#199=NEXT_ASSEMBLY_USAGE_OCCURRENCE(
'Linear Ball Bushing - 12 x 21 x 30 mm:3',
'Linear Ball Bushing - 12 x 21 x 30 mm:3',
'Linear Ball Bushing - 12 x 21 x 30 mm:3',#6589,#6592,
'Linear Ball Bushing - 12 x 21 x 30 mm:3');
#200=NEXT_ASSEMBLY_USAGE_OCCURRENCE('End retainer:2','End retainer:2',
'End retainer:2',#6589,#6595,'End retainer:2');
#201=NEXT_ASSEMBLY_USAGE_OCCURRENCE('End retainer:3','End retainer:3',
'End retainer:3',#6589,#6595,'End retainer:3');
#202=NEXT_ASSEMBLY_USAGE_OCCURRENCE('Cap Screw - M4x16:6',
'Cap Screw - M4x16:6','Cap Screw - M4x16:6',#6589,#6596,
'Cap Screw - M4x16:6');
#203=NEXT_ASSEMBLY_USAGE_OCCURRENCE('Cap Screw - M4x16:7',
'Cap Screw - M4x16:7','Cap Screw - M4x16:7',#6589,#6596,
'Cap Screw - M4x16:7');
#204=NEXT_ASSEMBLY_USAGE_OCCURRENCE('Cap Screw - M4x16:8',
'Cap Screw - M4x16:8','Cap Screw - M4x16:8',#6589,#6596,
'Cap Screw - M4x16:8');
#205=NEXT_ASSEMBLY_USAGE_OCCURRENCE('Cap Screw - M4x16:9',
'Cap Screw - M4x16:9','Cap Screw - M4x16:9',#6589,#6596,
'Cap Screw - M4x16:9');
#206=NEXT_ASSEMBLY_USAGE_OCCURRENCE('Cap Screw - M4x16:10',
'Cap Screw - M4x16:10','Cap Screw - M4x16:10',#6589,#6596,
'Cap Screw - M4x16:10');
#207=NEXT_ASSEMBLY_USAGE_OCCURRENCE('Cap Screw - M4x16:11',
'Cap Screw - M4x16:11','Cap Screw - M4x16:11',#6589,#6596,
'Cap Screw - M4x16:11');
#208=NEXT_ASSEMBLY_USAGE_OCCURRENCE('Cap Screw - M4x16:12',
'Cap Screw - M4x16:12','Cap Screw - M4x16:12',#6589,#6596,
'Cap Screw - M4x16:12');
#209=NEXT_ASSEMBLY_USAGE_OCCURRENCE('Cap Screw - M4x16:13',
'Cap Screw - M4x16:13','Cap Screw - M4x16:13',#6589,#6596,
'Cap Screw - M4x16:13');
#210=NEXT_ASSEMBLY_USAGE_OCCURRENCE('Cap Screw - M5x20:2',
'Cap Screw - M5x20:2','Cap Screw - M5x20:2',#6589,#6597,
'Cap Screw - M5x20:2');
#211=NEXT_ASSEMBLY_USAGE_OCCURRENCE('Cap Screw - M5x20:3',
'Cap Screw - M5x20:3','Cap Screw - M5x20:3',#6589,#6597,
'Cap Screw - M5x20:3');
#212=NEXT_ASSEMBLY_USAGE_OCCURRENCE('Cap Screw - M5x20:4',
'Cap Screw - M5x20:4','Cap Screw - M5x20:4',#6589,#6597,
'Cap Screw - M5x20:4');
#213=NEXT_ASSEMBLY_USAGE_OCCURRENCE('Cap Screw - M5x20:5',
'Cap Screw - M5x20:5','Cap Screw - M5x20:5',#6589,#6597,
'Cap Screw - M5x20:5');
#214=NEXT_ASSEMBLY_USAGE_OCCURRENCE('Grip:2','Grip:2','Grip:2',#6589,#6598,
'Grip:2');
#215=NEXT_ASSEMBLY_USAGE_OCCURRENCE('Flat Washer - M6:2',
'Flat Washer - M6:2','Flat Washer - M6:2',#6589,#6599,
'Flat Washer - M6:2');
#216=NEXT_ASSEMBLY_USAGE_OCCURRENCE('Cap Screw - M6x25:2',
'Cap Screw - M6x25:2','Cap Screw - M6x25:2',#6589,#6600,
'Cap Screw - M6x25:2');
#217=NEXT_ASSEMBLY_USAGE_OCCURRENCE('Shafts supports and end stops:1',
'Shafts supports and end stops:1','Shafts supports and end stops:1',#6581,
#6582,'Shafts supports and end stops:1');
#218=NEXT_ASSEMBLY_USAGE_OCCURRENCE('Two-bushing carriage:1',
'Two-bushing carriage:1','Two-bushing carriage:1',#6581,#6589,
'Two-bushing carriage:1');
#219=ORIENTED_CLOSED_SHELL('',*,#3641,.F.);
#220=ORIENTED_CLOSED_SHELL('',*,#3651,.F.);
#221=ORIENTED_CLOSED_SHELL('',*,#3653,.F.);
#222=ORIENTED_CLOSED_SHELL('',*,#3657,.F.);
#223=BREP_WITH_VOIDS('Body1',#3642,(#219));
#224=BREP_WITH_VOIDS('Body1',#3650,(#220));
#225=BREP_WITH_VOIDS('Body1',#3652,(#221));
#226=BREP_WITH_VOIDS('Body1',#3656,(#222));
#227=CONICAL_SURFACE('',#3881,0.55,0.785398163397448);
#228=CONICAL_SURFACE('',#3887,0.55,0.785398163397441);
#229=CONICAL_SURFACE('',#3941,0.4,0.785398163397448);
#230=CONICAL_SURFACE('',#3945,0.41,0.785398163397448);
#231=CONICAL_SURFACE('',#3949,0.26,0.463647609000806);
#232=CONICAL_SURFACE('',#4124,0.325,0.785398163397448);
#233=CONICAL_SURFACE('',#4128,0.335,0.785398163397448);
#234=CONICAL_SURFACE('',#4132,0.21,0.463647609000806);
#235=CONICAL_SURFACE('',#4136,0.18,0.785398163397448);
#236=CONICAL_SURFACE('',#4150,0.4,0.785398163397448);
#237=CONICAL_SURFACE('',#4154,0.41,0.785398163397448);
#238=CONICAL_SURFACE('',#4158,0.26,0.463647609000806);
#239=CONICAL_SURFACE('',#4162,0.225,0.785398163397448);
#240=CONICAL_SURFACE('',#4221,0.475,0.785398163397449);
#241=CONICAL_SURFACE('',#4225,0.485,0.785398163397448);
#242=CONICAL_SURFACE('',#4229,0.31,0.463647609000806);
#243=CONICAL_SURFACE('',#4233,0.27,0.785398163397448);
#244=SHAPE_REPRESENTATION_RELATIONSHIP('SRR','None',#6562,#260);
#245=SHAPE_REPRESENTATION_RELATIONSHIP('SRR','None',#6563,#261);
#246=SHAPE_REPRESENTATION_RELATIONSHIP('SRR','None',#6564,#262);
#247=SHAPE_REPRESENTATION_RELATIONSHIP('SRR','None',#6565,#263);
#248=SHAPE_REPRESENTATION_RELATIONSHIP('SRR','None',#6566,#264);
#249=SHAPE_REPRESENTATION_RELATIONSHIP('SRR','None',#6567,#265);
#250=SHAPE_REPRESENTATION_RELATIONSHIP('SRR','None',#6569,#266);
#251=SHAPE_REPRESENTATION_RELATIONSHIP('SRR','None',#6570,#267);
#252=SHAPE_REPRESENTATION_RELATIONSHIP('SRR','None',#6572,#268);
#253=SHAPE_REPRESENTATION_RELATIONSHIP('SRR','None',#6573,#269);
#254=SHAPE_REPRESENTATION_RELATIONSHIP('SRR','None',#6574,#270);
#255=SHAPE_REPRESENTATION_RELATIONSHIP('SRR','None',#6575,#271);
#256=SHAPE_REPRESENTATION_RELATIONSHIP('SRR','None',#6576,#272);
#257=SHAPE_REPRESENTATION_RELATIONSHIP('SRR','None',#6577,#273);
#258=SHAPE_REPRESENTATION_RELATIONSHIP('SRR','None',#6578,#274);
#259=SHAPE_REPRESENTATION_RELATIONSHIP('SRR','None',#6579,#275);
#260=ADVANCED_BREP_SHAPE_REPRESENTATION('',(#292),#6445);
#261=ADVANCED_BREP_SHAPE_REPRESENTATION('',(#293),#6446);
#262=ADVANCED_BREP_SHAPE_REPRESENTATION('',(#294),#6447);
#263=ADVANCED_BREP_SHAPE_REPRESENTATION('',(#223),#6448);
#264=ADVANCED_BREP_SHAPE_REPRESENTATION('',(#295),#6449);
#265=ADVANCED_BREP_SHAPE_REPRESENTATION('',(#296),#6450);
#266=ADVANCED_BREP_SHAPE_REPRESENTATION('',(#297),#6452);
#267=ADVANCED_BREP_SHAPE_REPRESENTATION('',(#298),#6453);
#268=ADVANCED_BREP_SHAPE_REPRESENTATION('',(#299),#6455);
#269=ADVANCED_BREP_SHAPE_REPRESENTATION('',(#300),#6456);
#270=ADVANCED_BREP_SHAPE_REPRESENTATION('',(#301),#6457);
#271=ADVANCED_BREP_SHAPE_REPRESENTATION('',(#224),#6458);
#272=ADVANCED_BREP_SHAPE_REPRESENTATION('',(#225),#6459);
#273=ADVANCED_BREP_SHAPE_REPRESENTATION('',(#302),#6460);
#274=ADVANCED_BREP_SHAPE_REPRESENTATION('',(#303),#6461);
#275=ADVANCED_BREP_SHAPE_REPRESENTATION('',(#226),#6462);
#276=STYLED_ITEM('',(#6719),#292);
#277=STYLED_ITEM('',(#6740),#293);
#278=STYLED_ITEM('',(#6740),#294);
#279=STYLED_ITEM('',(#6747),#223);
#280=STYLED_ITEM('',(#6733),#295);
#281=STYLED_ITEM('',(#6754),#296);
#282=STYLED_ITEM('',(#6719),#297);
#283=STYLED_ITEM('',(#6733),#298);
#284=STYLED_ITEM('',(#6754),#299);
#285=STYLED_ITEM('',(#6733),#300);
#286=STYLED_ITEM('',(#6726),#301);
#287=STYLED_ITEM('',(#6747),#224);
#288=STYLED_ITEM('',(#6747),#225);
#289=STYLED_ITEM('',(#6747),#302);
#290=STYLED_ITEM('',(#6747),#303);
#291=STYLED_ITEM('',(#6747),#226);
#292=MANIFOLD_SOLID_BREP('Body1',#3638);
#293=MANIFOLD_SOLID_BREP('Body1',#3639);
#294=MANIFOLD_SOLID_BREP('Body1',#3640);
#295=MANIFOLD_SOLID_BREP('Body1',#3643);
#296=MANIFOLD_SOLID_BREP('Body1',#3644);
#297=MANIFOLD_SOLID_BREP('Body1',#3645);
#298=MANIFOLD_SOLID_BREP('Body1',#3646);
#299=MANIFOLD_SOLID_BREP('Body1',#3647);
#300=MANIFOLD_SOLID_BREP('Body1',#3648);
#301=MANIFOLD_SOLID_BREP('Body1',#3649);
#302=MANIFOLD_SOLID_BREP('Body1',#3654);
#303=MANIFOLD_SOLID_BREP('Body1',#3655);
#304=FACE_BOUND('',#750,.T.);
#305=FACE_BOUND('',#751,.T.);
#306=FACE_BOUND('',#752,.T.);
#307=FACE_BOUND('',#753,.T.);
#308=FACE_BOUND('',#754,.T.);
#309=FACE_BOUND('',#755,.T.);
#310=FACE_BOUND('',#756,.T.);
#311=FACE_BOUND('',#757,.T.);
#312=FACE_BOUND('',#758,.T.);
#313=FACE_BOUND('',#759,.T.);
#314=FACE_BOUND('',#760,.T.);
#315=FACE_BOUND('',#761,.T.);
#316=FACE_BOUND('',#763,.T.);
#317=FACE_BOUND('',#764,.T.);
#318=FACE_BOUND('',#765,.T.);
#319=FACE_BOUND('',#766,.T.);
#320=FACE_BOUND('',#767,.T.);
#321=FACE_BOUND('',#768,.T.);
#322=FACE_BOUND('',#769,.T.);
#323=FACE_BOUND('',#770,.T.);
#324=FACE_BOUND('',#771,.T.);
#325=FACE_BOUND('',#772,.T.);
#326=FACE_BOUND('',#773,.T.);
#327=FACE_BOUND('',#774,.T.);
#328=FACE_BOUND('',#785,.T.);
#329=FACE_BOUND('',#787,.T.);
#330=FACE_BOUND('',#789,.T.);
#331=FACE_BOUND('',#796,.T.);
#332=FACE_BOUND('',#799,.T.);
#333=FACE_BOUND('',#800,.T.);
#334=FACE_BOUND('',#803,.T.);
#335=FACE_BOUND('',#806,.T.);
#336=FACE_BOUND('',#809,.T.);
#337=FACE_BOUND('',#812,.T.);
#338=FACE_BOUND('',#827,.T.);
#339=FACE_BOUND('',#832,.T.);
#340=FACE_BOUND('',#835,.T.);
#341=FACE_BOUND('',#843,.T.);
#342=FACE_BOUND('',#844,.T.);
#343=FACE_BOUND('',#846,.T.);
#344=FACE_BOUND('',#847,.T.);
#345=FACE_BOUND('',#870,.T.);
#346=FACE_BOUND('',#871,.T.);
#347=FACE_BOUND('',#872,.T.);
#348=FACE_BOUND('',#873,.T.);
#349=FACE_BOUND('',#874,.T.);
#350=FACE_BOUND('',#875,.T.);
#351=FACE_BOUND('',#878,.T.);
#352=FACE_BOUND('',#879,.T.);
#353=FACE_BOUND('',#880,.T.);
#354=FACE_BOUND('',#881,.T.);
#355=FACE_BOUND('',#882,.T.);
#356=FACE_BOUND('',#883,.T.);
#357=FACE_BOUND('',#885,.T.);
#358=FACE_BOUND('',#886,.T.);
#359=FACE_BOUND('',#887,.T.);
#360=FACE_BOUND('',#888,.T.);
#361=FACE_BOUND('',#900,.T.);
#362=FACE_BOUND('',#901,.T.);
#363=FACE_BOUND('',#902,.T.);
#364=FACE_BOUND('',#903,.T.);
#365=FACE_BOUND('',#904,.T.);
#366=FACE_BOUND('',#906,.T.);
#367=FACE_BOUND('',#907,.T.);
#368=FACE_BOUND('',#908,.T.);
#369=FACE_BOUND('',#909,.T.);
#370=FACE_BOUND('',#910,.T.);
#371=FACE_BOUND('',#917,.T.);
#372=FACE_BOUND('',#920,.T.);
#373=FACE_BOUND('',#923,.T.);
#374=FACE_BOUND('',#926,.T.);
#375=FACE_BOUND('',#929,.T.);
#376=FACE_BOUND('',#932,.T.);
#377=FACE_BOUND('',#934,.T.);
#378=FACE_BOUND('',#940,.T.);
#379=FACE_BOUND('',#942,.T.);
#380=FACE_BOUND('',#944,.T.);
#381=FACE_BOUND('',#946,.T.);
#382=FACE_BOUND('',#955,.T.);
#383=FACE_BOUND('',#956,.T.);
#384=FACE_BOUND('',#957,.T.);
#385=FACE_BOUND('',#958,.T.);
#386=FACE_BOUND('',#959,.T.);
#387=FACE_BOUND('',#960,.T.);
#388=FACE_BOUND('',#963,.T.);
#389=FACE_BOUND('',#964,.T.);
#390=FACE_BOUND('',#965,.T.);
#391=FACE_BOUND('',#966,.T.);
#392=FACE_BOUND('',#967,.T.);
#393=FACE_BOUND('',#968,.T.);
#394=FACE_BOUND('',#976,.T.);
#395=FACE_BOUND('',#994,.T.);
#396=FACE_BOUND('',#1010,.T.);
#397=FACE_BOUND('',#1012,.T.);
#398=FACE_BOUND('',#1016,.T.);
#399=FACE_BOUND('',#1018,.T.);
#400=FACE_BOUND('',#1024,.T.);
#401=PLANE('',#3874);
#402=PLANE('',#3875);
#403=PLANE('',#3876);
#404=PLANE('',#3877);
#405=PLANE('',#3878);
#406=PLANE('',#3879);
#407=PLANE('',#3886);
#408=PLANE('',#3889);
#409=PLANE('',#3891);
#410=PLANE('',#3898);
#411=PLANE('',#3899);
#412=PLANE('',#3901);
#413=PLANE('',#3903);
#414=PLANE('',#3917);
#415=PLANE('',#3918);
#416=PLANE('',#3919);
#417=PLANE('',#3920);
#418=PLANE('',#3921);
#419=PLANE('',#3922);
#420=PLANE('',#3923);
#421=PLANE('',#3924);
#422=PLANE('',#3925);
#423=PLANE('',#3926);
#424=PLANE('',#3927);
#425=PLANE('',#3929);
#426=PLANE('',#3930);
#427=PLANE('',#3931);
#428=PLANE('',#3932);
#429=PLANE('',#3933);
#430=PLANE('',#3934);
#431=PLANE('',#3935);
#432=PLANE('',#3936);
#433=PLANE('',#3937);
#434=PLANE('',#3939);
#435=PLANE('',#3947);
#436=PLANE('',#3956);
#437=PLANE('',#3961);
#438=PLANE('',#3967);
#439=PLANE('',#3968);
#440=PLANE('',#3969);
#441=PLANE('',#3970);
#442=PLANE('',#3971);
#443=PLANE('',#3972);
#444=PLANE('',#3974);
#445=PLANE('',#3975);
#446=PLANE('',#3976);
#447=PLANE('',#3977);
#448=PLANE('',#3978);
#449=PLANE('',#3979);
#450=PLANE('',#3997);
#451=PLANE('',#4001);
#452=PLANE('',#4005);
#453=PLANE('',#4009);
#454=PLANE('',#4016);
#455=PLANE('',#4017);
#456=PLANE('',#4018);
#457=PLANE('',#4019);
#458=PLANE('',#4020);
#459=PLANE('',#4021);
#460=PLANE('',#4038);
#461=PLANE('',#4039);
#462=PLANE('',#4040);
#463=PLANE('',#4041);
#464=PLANE('',#4042);
#465=PLANE('',#4043);
#466=PLANE('',#4046);
#467=PLANE('',#4048);
#468=PLANE('',#4049);
#469=PLANE('',#4051);
#470=PLANE('',#4052);
#471=PLANE('',#4053);
#472=PLANE('',#4058);
#473=PLANE('',#4062);
#474=PLANE('',#4066);
#475=PLANE('',#4070);
#476=PLANE('',#4074);
#477=PLANE('',#4078);
#478=PLANE('',#4081);
#479=PLANE('',#4082);
#480=PLANE('',#4085);
#481=PLANE('',#4086);
#482=PLANE('',#4091);
#483=PLANE('',#4115);
#484=PLANE('',#4116);
#485=PLANE('',#4117);
#486=PLANE('',#4118);
#487=PLANE('',#4119);
#488=PLANE('',#4120);
#489=PLANE('',#4122);
#490=PLANE('',#4130);
#491=PLANE('',#4138);
#492=PLANE('',#4139);
#493=PLANE('',#4140);
#494=PLANE('',#4141);
#495=PLANE('',#4142);
#496=PLANE('',#4143);
#497=PLANE('',#4144);
#498=PLANE('',#4145);
#499=PLANE('',#4146);
#500=PLANE('',#4148);
#501=PLANE('',#4156);
#502=PLANE('',#4164);
#503=PLANE('',#4165);
#504=PLANE('',#4166);
#505=PLANE('',#4167);
#506=PLANE('',#4168);
#507=PLANE('',#4169);
#508=PLANE('',#4170);
#509=PLANE('',#4171);
#510=PLANE('',#4172);
#511=PLANE('',#4207);
#512=PLANE('',#4208);
#513=PLANE('',#4216);
#514=PLANE('',#4217);
#515=PLANE('',#4219);
#516=PLANE('',#4227);
#517=PLANE('',#4235);
#518=PLANE('',#4236);
#519=PLANE('',#4237);
#520=PLANE('',#4238);
#521=PLANE('',#4239);
#522=PLANE('',#4240);
#523=PLANE('',#4241);
#524=PLANE('',#4242);
#525=PLANE('',#4243);
#526=FACE_OUTER_BOUND('',#733,.T.);
#527=FACE_OUTER_BOUND('',#734,.T.);
#528=FACE_OUTER_BOUND('',#735,.T.);
#529=FACE_OUTER_BOUND('',#736,.T.);
#530=FACE_OUTER_BOUND('',#737,.T.);
#531=FACE_OUTER_BOUND('',#738,.T.);
#532=FACE_OUTER_BOUND('',#739,.T.);
#533=FACE_OUTER_BOUND('',#740,.T.);
#534=FACE_OUTER_BOUND('',#741,.T.);
#535=FACE_OUTER_BOUND('',#742,.T.);
#536=FACE_OUTER_BOUND('',#743,.T.);
#537=FACE_OUTER_BOUND('',#744,.T.);
#538=FACE_OUTER_BOUND('',#745,.T.);
#539=FACE_OUTER_BOUND('',#746,.T.);
#540=FACE_OUTER_BOUND('',#747,.T.);
#541=FACE_OUTER_BOUND('',#748,.T.);
#542=FACE_OUTER_BOUND('',#749,.T.);
#543=FACE_OUTER_BOUND('',#762,.T.);
#544=FACE_OUTER_BOUND('',#775,.T.);
#545=FACE_OUTER_BOUND('',#776,.T.);
#546=FACE_OUTER_BOUND('',#777,.T.);
#547=FACE_OUTER_BOUND('',#778,.T.);
#548=FACE_OUTER_BOUND('',#779,.T.);
#549=FACE_OUTER_BOUND('',#780,.T.);
#550=FACE_OUTER_BOUND('',#781,.T.);
#551=FACE_OUTER_BOUND('',#782,.T.);
#552=FACE_OUTER_BOUND('',#783,.T.);
#553=FACE_OUTER_BOUND('',#784,.T.);
#554=FACE_OUTER_BOUND('',#786,.T.);
#555=FACE_OUTER_BOUND('',#788,.T.);
#556=FACE_OUTER_BOUND('',#790,.T.);
#557=FACE_OUTER_BOUND('',#791,.T.);
#558=FACE_OUTER_BOUND('',#792,.T.);
#559=FACE_OUTER_BOUND('',#793,.T.);
#560=FACE_OUTER_BOUND('',#794,.T.);
#561=FACE_OUTER_BOUND('',#795,.T.);
#562=FACE_OUTER_BOUND('',#797,.T.);
#563=FACE_OUTER_BOUND('',#798,.T.);
#564=FACE_OUTER_BOUND('',#801,.T.);
#565=FACE_OUTER_BOUND('',#802,.T.);
#566=FACE_OUTER_BOUND('',#804,.T.);
#567=FACE_OUTER_BOUND('',#805,.T.);
#568=FACE_OUTER_BOUND('',#807,.T.);
#569=FACE_OUTER_BOUND('',#808,.T.);
#570=FACE_OUTER_BOUND('',#810,.T.);
#571=FACE_OUTER_BOUND('',#811,.T.);
#572=FACE_OUTER_BOUND('',#813,.T.);
#573=FACE_OUTER_BOUND('',#814,.T.);
#574=FACE_OUTER_BOUND('',#815,.T.);
#575=FACE_OUTER_BOUND('',#816,.T.);
#576=FACE_OUTER_BOUND('',#817,.T.);
#577=FACE_OUTER_BOUND('',#818,.T.);
#578=FACE_OUTER_BOUND('',#819,.T.);
#579=FACE_OUTER_BOUND('',#820,.T.);
#580=FACE_OUTER_BOUND('',#821,.T.);
#581=FACE_OUTER_BOUND('',#822,.T.);
#582=FACE_OUTER_BOUND('',#823,.T.);
#583=FACE_OUTER_BOUND('',#824,.T.);
#584=FACE_OUTER_BOUND('',#825,.T.);
#585=FACE_OUTER_BOUND('',#826,.T.);
#586=FACE_OUTER_BOUND('',#828,.T.);
#587=FACE_OUTER_BOUND('',#829,.T.);
#588=FACE_OUTER_BOUND('',#830,.T.);
#589=FACE_OUTER_BOUND('',#831,.T.);
#590=FACE_OUTER_BOUND('',#833,.T.);
#591=FACE_OUTER_BOUND('',#834,.T.);
#592=FACE_OUTER_BOUND('',#836,.T.);
#593=FACE_OUTER_BOUND('',#837,.T.);
#594=FACE_OUTER_BOUND('',#838,.T.);
#595=FACE_OUTER_BOUND('',#839,.T.);
#596=FACE_OUTER_BOUND('',#840,.T.);
#597=FACE_OUTER_BOUND('',#841,.T.);
#598=FACE_OUTER_BOUND('',#842,.T.);
#599=FACE_OUTER_BOUND('',#845,.T.);
#600=FACE_OUTER_BOUND('',#848,.T.);
#601=FACE_OUTER_BOUND('',#849,.T.);
#602=FACE_OUTER_BOUND('',#850,.T.);
#603=FACE_OUTER_BOUND('',#851,.T.);
#604=FACE_OUTER_BOUND('',#852,.T.);
#605=FACE_OUTER_BOUND('',#853,.T.);
#606=FACE_OUTER_BOUND('',#854,.T.);
#607=FACE_OUTER_BOUND('',#855,.T.);
#608=FACE_OUTER_BOUND('',#856,.T.);
#609=FACE_OUTER_BOUND('',#857,.T.);
#610=FACE_OUTER_BOUND('',#858,.T.);
#611=FACE_OUTER_BOUND('',#859,.T.);
#612=FACE_OUTER_BOUND('',#860,.T.);
#613=FACE_OUTER_BOUND('',#861,.T.);
#614=FACE_OUTER_BOUND('',#862,.T.);
#615=FACE_OUTER_BOUND('',#863,.T.);
#616=FACE_OUTER_BOUND('',#864,.T.);
#617=FACE_OUTER_BOUND('',#865,.T.);
#618=FACE_OUTER_BOUND('',#866,.T.);
#619=FACE_OUTER_BOUND('',#867,.T.);
#620=FACE_OUTER_BOUND('',#868,.T.);
#621=FACE_OUTER_BOUND('',#869,.T.);
#622=FACE_OUTER_BOUND('',#876,.T.);
#623=FACE_OUTER_BOUND('',#877,.T.);
#624=FACE_OUTER_BOUND('',#884,.T.);
#625=FACE_OUTER_BOUND('',#889,.T.);
#626=FACE_OUTER_BOUND('',#890,.T.);
#627=FACE_OUTER_BOUND('',#891,.T.);
#628=FACE_OUTER_BOUND('',#892,.T.);
#629=FACE_OUTER_BOUND('',#893,.T.);
#630=FACE_OUTER_BOUND('',#894,.T.);
#631=FACE_OUTER_BOUND('',#895,.T.);
#632=FACE_OUTER_BOUND('',#896,.T.);
#633=FACE_OUTER_BOUND('',#897,.T.);
#634=FACE_OUTER_BOUND('',#898,.T.);
#635=FACE_OUTER_BOUND('',#899,.T.);
#636=FACE_OUTER_BOUND('',#905,.T.);
#637=FACE_OUTER_BOUND('',#911,.T.);
#638=FACE_OUTER_BOUND('',#912,.T.);
#639=FACE_OUTER_BOUND('',#913,.T.);
#640=FACE_OUTER_BOUND('',#914,.T.);
#641=FACE_OUTER_BOUND('',#915,.T.);
#642=FACE_OUTER_BOUND('',#916,.T.);
#643=FACE_OUTER_BOUND('',#918,.T.);
#644=FACE_OUTER_BOUND('',#919,.T.);
#645=FACE_OUTER_BOUND('',#921,.T.);
#646=FACE_OUTER_BOUND('',#922,.T.);
#647=FACE_OUTER_BOUND('',#924,.T.);
#648=FACE_OUTER_BOUND('',#925,.T.);
#649=FACE_OUTER_BOUND('',#927,.T.);
#650=FACE_OUTER_BOUND('',#928,.T.);
#651=FACE_OUTER_BOUND('',#930,.T.);
#652=FACE_OUTER_BOUND('',#931,.T.);
#653=FACE_OUTER_BOUND('',#933,.T.);
#654=FACE_OUTER_BOUND('',#935,.T.);
#655=FACE_OUTER_BOUND('',#936,.T.);
#656=FACE_OUTER_BOUND('',#937,.T.);
#657=FACE_OUTER_BOUND('',#938,.T.);
#658=FACE_OUTER_BOUND('',#939,.T.);
#659=FACE_OUTER_BOUND('',#941,.T.);
#660=FACE_OUTER_BOUND('',#943,.T.);
#661=FACE_OUTER_BOUND('',#945,.T.);
#662=FACE_OUTER_BOUND('',#947,.T.);
#663=FACE_OUTER_BOUND('',#948,.T.);
#664=FACE_OUTER_BOUND('',#949,.T.);
#665=FACE_OUTER_BOUND('',#950,.T.);
#666=FACE_OUTER_BOUND('',#951,.T.);
#667=FACE_OUTER_BOUND('',#952,.T.);
#668=FACE_OUTER_BOUND('',#953,.T.);
#669=FACE_OUTER_BOUND('',#954,.T.);
#670=FACE_OUTER_BOUND('',#961,.T.);
#671=FACE_OUTER_BOUND('',#962,.T.);
#672=FACE_OUTER_BOUND('',#969,.T.);
#673=FACE_OUTER_BOUND('',#970,.T.);
#674=FACE_OUTER_BOUND('',#971,.T.);
#675=FACE_OUTER_BOUND('',#972,.T.);
#676=FACE_OUTER_BOUND('',#973,.T.);
#677=FACE_OUTER_BOUND('',#974,.T.);
#678=FACE_OUTER_BOUND('',#975,.T.);
#679=FACE_OUTER_BOUND('',#977,.T.);
#680=FACE_OUTER_BOUND('',#978,.T.);
#681=FACE_OUTER_BOUND('',#979,.T.);
#682=FACE_OUTER_BOUND('',#980,.T.);
#683=FACE_OUTER_BOUND('',#981,.T.);
#684=FACE_OUTER_BOUND('',#982,.T.);
#685=FACE_OUTER_BOUND('',#983,.T.);
#686=FACE_OUTER_BOUND('',#984,.T.);
#687=FACE_OUTER_BOUND('',#985,.T.);
#688=FACE_OUTER_BOUND('',#986,.T.);
#689=FACE_OUTER_BOUND('',#987,.T.);
#690=FACE_OUTER_BOUND('',#988,.T.);
#691=FACE_OUTER_BOUND('',#989,.T.);
#692=FACE_OUTER_BOUND('',#990,.T.);
#693=FACE_OUTER_BOUND('',#991,.T.);
#694=FACE_OUTER_BOUND('',#992,.T.);
#695=FACE_OUTER_BOUND('',#993,.T.);
#696=FACE_OUTER_BOUND('',#995,.T.);
#697=FACE_OUTER_BOUND('',#996,.T.);
#698=FACE_OUTER_BOUND('',#997,.T.);
#699=FACE_OUTER_BOUND('',#998,.T.);
#700=FACE_OUTER_BOUND('',#999,.T.);
#701=FACE_OUTER_BOUND('',#1000,.T.);
#702=FACE_OUTER_BOUND('',#1001,.T.);
#703=FACE_OUTER_BOUND('',#1002,.T.);
#704=FACE_OUTER_BOUND('',#1003,.T.);
#705=FACE_OUTER_BOUND('',#1004,.T.);
#706=FACE_OUTER_BOUND('',#1005,.T.);
#707=FACE_OUTER_BOUND('',#1006,.T.);
#708=FACE_OUTER_BOUND('',#1007,.T.);
#709=FACE_OUTER_BOUND('',#1008,.T.);
#710=FACE_OUTER_BOUND('',#1009,.T.);
#711=FACE_OUTER_BOUND('',#1011,.T.);
#712=FACE_OUTER_BOUND('',#1013,.T.);
#713=FACE_OUTER_BOUND('',#1014,.T.);
#714=FACE_OUTER_BOUND('',#1015,.T.);
#715=FACE_OUTER_BOUND('',#1017,.T.);
#716=FACE_OUTER_BOUND('',#1019,.T.);
#717=FACE_OUTER_BOUND('',#1020,.T.);
#718=FACE_OUTER_BOUND('',#1021,.T.);
#719=FACE_OUTER_BOUND('',#1022,.T.);
#720=FACE_OUTER_BOUND('',#1023,.T.);
#721=FACE_OUTER_BOUND('',#1025,.T.);
#722=FACE_OUTER_BOUND('',#1026,.T.);
#723=FACE_OUTER_BOUND('',#1027,.T.);
#724=FACE_OUTER_BOUND('',#1028,.T.);
#725=FACE_OUTER_BOUND('',#1029,.T.);
#726=FACE_OUTER_BOUND('',#1030,.T.);
#727=FACE_OUTER_BOUND('',#1031,.T.);
#728=FACE_OUTER_BOUND('',#1032,.T.);
#729=FACE_OUTER_BOUND('',#1033,.T.);
#730=FACE_OUTER_BOUND('',#1034,.T.);
#731=FACE_OUTER_BOUND('',#1035,.T.);
#732=FACE_OUTER_BOUND('',#1036,.T.);
#733=EDGE_LOOP('',(#2488,#2489,#2490,#2491));
#734=EDGE_LOOP('',(#2492,#2493,#2494,#2495));
#735=EDGE_LOOP('',(#2496,#2497,#2498,#2499));
#736=EDGE_LOOP('',(#2500,#2501,#2502,#2503));
#737=EDGE_LOOP('',(#2504,#2505,#2506,#2507));
#738=EDGE_LOOP('',(#2508,#2509,#2510,#2511));
#739=EDGE_LOOP('',(#2512,#2513,#2514,#2515));
#740=EDGE_LOOP('',(#2516,#2517,#2518,#2519));
#741=EDGE_LOOP('',(#2520,#2521,#2522,#2523));
#742=EDGE_LOOP('',(#2524,#2525,#2526,#2527));
#743=EDGE_LOOP('',(#2528,#2529,#2530,#2531));
#744=EDGE_LOOP('',(#2532,#2533,#2534,#2535));
#745=EDGE_LOOP('',(#2536,#2537,#2538,#2539));
#746=EDGE_LOOP('',(#2540,#2541,#2542,#2543));
#747=EDGE_LOOP('',(#2544,#2545,#2546,#2547));
#748=EDGE_LOOP('',(#2548,#2549,#2550,#2551));
#749=EDGE_LOOP('',(#2552,#2553,#2554,#2555));
#750=EDGE_LOOP('',(#2556));
#751=EDGE_LOOP('',(#2557));
#752=EDGE_LOOP('',(#2558));
#753=EDGE_LOOP('',(#2559));
#754=EDGE_LOOP('',(#2560));
#755=EDGE_LOOP('',(#2561));
#756=EDGE_LOOP('',(#2562));
#757=EDGE_LOOP('',(#2563));
#758=EDGE_LOOP('',(#2564));
#759=EDGE_LOOP('',(#2565));
#760=EDGE_LOOP('',(#2566));
#761=EDGE_LOOP('',(#2567));
#762=EDGE_LOOP('',(#2568,#2569,#2570,#2571));
#763=EDGE_LOOP('',(#2572));
#764=EDGE_LOOP('',(#2573));
#765=EDGE_LOOP('',(#2574));
#766=EDGE_LOOP('',(#2575));
#767=EDGE_LOOP('',(#2576));
#768=EDGE_LOOP('',(#2577));
#769=EDGE_LOOP('',(#2578));
#770=EDGE_LOOP('',(#2579));
#771=EDGE_LOOP('',(#2580));
#772=EDGE_LOOP('',(#2581));
#773=EDGE_LOOP('',(#2582));
#774=EDGE_LOOP('',(#2583));
#775=EDGE_LOOP('',(#2584,#2585,#2586,#2587));
#776=EDGE_LOOP('',(#2588,#2589,#2590,#2591));
#777=EDGE_LOOP('',(#2592));
#778=EDGE_LOOP('',(#2593,#2594,#2595,#2596));
#779=EDGE_LOOP('',(#2597));
#780=EDGE_LOOP('',(#2598,#2599));
#781=EDGE_LOOP('',(#2600,#2601,#2602,#2603));
#782=EDGE_LOOP('',(#2604,#2605,#2606,#2607));
#783=EDGE_LOOP('',(#2608,#2609));
#784=EDGE_LOOP('',(#2610,#2611,#2612,#2613,#2614,#2615));
#785=EDGE_LOOP('',(#2616));
#786=EDGE_LOOP('',(#2617,#2618,#2619,#2620,#2621,#2622,#2623,#2624));
#787=EDGE_LOOP('',(#2625));
#788=EDGE_LOOP('',(#2626,#2627,#2628,#2629,#2630,#2631));
#789=EDGE_LOOP('',(#2632));
#790=EDGE_LOOP('',(#2633,#2634,#2635,#2636));
#791=EDGE_LOOP('',(#2637,#2638,#2639,#2640));
#792=EDGE_LOOP('',(#2641,#2642,#2643,#2644));
#793=EDGE_LOOP('',(#2645,#2646,#2647,#2648));
#794=EDGE_LOOP('',(#2649,#2650,#2651,#2652));
#795=EDGE_LOOP('',(#2653,#2654,#2655,#2656,#2657,#2658,#2659,#2660,#2661,
#2662,#2663,#2664));
#796=EDGE_LOOP('',(#2665));
#797=EDGE_LOOP('',(#2666,#2667,#2668,#2669));
#798=EDGE_LOOP('',(#2670,#2671,#2672,#2673));
#799=EDGE_LOOP('',(#2674));
#800=EDGE_LOOP('',(#2675));
#801=EDGE_LOOP('',(#2676,#2677,#2678,#2679));
#802=EDGE_LOOP('',(#2680,#2681,#2682,#2683,#2684,#2685,#2686,#2687));
#803=EDGE_LOOP('',(#2688));
#804=EDGE_LOOP('',(#2689,#2690,#2691,#2692));
#805=EDGE_LOOP('',(#2693,#2694,#2695,#2696));
#806=EDGE_LOOP('',(#2697));
#807=EDGE_LOOP('',(#2698,#2699,#2700,#2701));
#808=EDGE_LOOP('',(#2702,#2703,#2704,#2705));
#809=EDGE_LOOP('',(#2706));
#810=EDGE_LOOP('',(#2707,#2708,#2709,#2710));
#811=EDGE_LOOP('',(#2711,#2712,#2713,#2714,#2715,#2716,#2717,#2718,#2719,
#2720,#2721,#2722));
#812=EDGE_LOOP('',(#2723));
#813=EDGE_LOOP('',(#2724,#2725,#2726,#2727));
#814=EDGE_LOOP('',(#2728,#2729,#2730,#2731));
#815=EDGE_LOOP('',(#2732,#2733,#2734,#2735));
#816=EDGE_LOOP('',(#2736,#2737,#2738,#2739));
#817=EDGE_LOOP('',(#2740,#2741,#2742,#2743));
#818=EDGE_LOOP('',(#2744,#2745,#2746,#2747));
#819=EDGE_LOOP('',(#2748,#2749,#2750,#2751,#2752,#2753));
#820=EDGE_LOOP('',(#2754,#2755,#2756,#2757,#2758,#2759));
#821=EDGE_LOOP('',(#2760));
#822=EDGE_LOOP('',(#2761));
#823=EDGE_LOOP('',(#2762,#2763,#2764,#2765));
#824=EDGE_LOOP('',(#2766,#2767,#2768,#2769));
#825=EDGE_LOOP('',(#2770,#2771,#2772,#2773));
#826=EDGE_LOOP('',(#2774));
#827=EDGE_LOOP('',(#2775));
#828=EDGE_LOOP('',(#2776,#2777,#2778,#2779));
#829=EDGE_LOOP('',(#2780,#2781,#2782,#2783));
#830=EDGE_LOOP('',(#2784,#2785,#2786,#2787));
#831=EDGE_LOOP('',(#2788));
#832=EDGE_LOOP('',(#2789));
#833=EDGE_LOOP('',(#2790,#2791,#2792,#2793));
#834=EDGE_LOOP('',(#2794));
#835=EDGE_LOOP('',(#2795));
#836=EDGE_LOOP('',(#2796,#2797,#2798,#2799));
#837=EDGE_LOOP('',(#2800,#2801,#2802,#2803));
#838=EDGE_LOOP('',(#2804,#2805,#2806,#2807));
#839=EDGE_LOOP('',(#2808,#2809,#2810,#2811));
#840=EDGE_LOOP('',(#2812,#2813,#2814,#2815));
#841=EDGE_LOOP('',(#2816,#2817,#2818,#2819));
#842=EDGE_LOOP('',(#2820,#2821,#2822,#2823));
#843=EDGE_LOOP('',(#2824));
#844=EDGE_LOOP('',(#2825));
#845=EDGE_LOOP('',(#2826,#2827,#2828,#2829));
#846=EDGE_LOOP('',(#2830));
#847=EDGE_LOOP('',(#2831));
#848=EDGE_LOOP('',(#2832,#2833,#2834,#2835));
#849=EDGE_LOOP('',(#2836,#2837,#2838,#2839));
#850=EDGE_LOOP('',(#2840,#2841,#2842,#2843));
#851=EDGE_LOOP('',(#2844,#2845,#2846,#2847));
#852=EDGE_LOOP('',(#2848,#2849,#2850,#2851));
#853=EDGE_LOOP('',(#2852,#2853,#2854,#2855));
#854=EDGE_LOOP('',(#2856,#2857,#2858,#2859));
#855=EDGE_LOOP('',(#2860,#2861,#2862,#2863));
#856=EDGE_LOOP('',(#2864,#2865,#2866,#2867));
#857=EDGE_LOOP('',(#2868,#2869,#2870,#2871));
#858=EDGE_LOOP('',(#2872,#2873,#2874,#2875));
#859=EDGE_LOOP('',(#2876));
#860=EDGE_LOOP('',(#2877,#2878,#2879,#2880));
#861=EDGE_LOOP('',(#2881));
#862=EDGE_LOOP('',(#2882,#2883,#2884,#2885));
#863=EDGE_LOOP('',(#2886));
#864=EDGE_LOOP('',(#2887,#2888,#2889,#2890));
#865=EDGE_LOOP('',(#2891));
#866=EDGE_LOOP('',(#2892,#2893,#2894,#2895));
#867=EDGE_LOOP('',(#2896,#2897,#2898,#2899));
#868=EDGE_LOOP('',(#2900,#2901,#2902,#2903));
#869=EDGE_LOOP('',(#2904,#2905,#2906,#2907));
#870=EDGE_LOOP('',(#2908));
#871=EDGE_LOOP('',(#2909));
#872=EDGE_LOOP('',(#2910));
#873=EDGE_LOOP('',(#2911));
#874=EDGE_LOOP('',(#2912));
#875=EDGE_LOOP('',(#2913));
#876=EDGE_LOOP('',(#2914,#2915,#2916,#2917));
#877=EDGE_LOOP('',(#2918,#2919,#2920,#2921));
#878=EDGE_LOOP('',(#2922));
#879=EDGE_LOOP('',(#2923));
#880=EDGE_LOOP('',(#2924));
#881=EDGE_LOOP('',(#2925));
#882=EDGE_LOOP('',(#2926));
#883=EDGE_LOOP('',(#2927));
#884=EDGE_LOOP('',(#2928,#2929,#2930,#2931));
#885=EDGE_LOOP('',(#2932));
#886=EDGE_LOOP('',(#2933));
#887=EDGE_LOOP('',(#2934));
#888=EDGE_LOOP('',(#2935));
#889=EDGE_LOOP('',(#2936,#2937,#2938,#2939));
#890=EDGE_LOOP('',(#2940,#2941,#2942,#2943));
#891=EDGE_LOOP('',(#2944,#2945,#2946,#2947));
#892=EDGE_LOOP('',(#2948,#2949,#2950,#2951));
#893=EDGE_LOOP('',(#2952,#2953,#2954,#2955));
#894=EDGE_LOOP('',(#2956,#2957,#2958,#2959));
#895=EDGE_LOOP('',(#2960,#2961,#2962,#2963));
#896=EDGE_LOOP('',(#2964,#2965,#2966,#2967));
#897=EDGE_LOOP('',(#2968,#2969,#2970,#2971));
#898=EDGE_LOOP('',(#2972,#2973,#2974,#2975));
#899=EDGE_LOOP('',(#2976,#2977,#2978,#2979));
#900=EDGE_LOOP('',(#2980));
#901=EDGE_LOOP('',(#2981));
#902=EDGE_LOOP('',(#2982));
#903=EDGE_LOOP('',(#2983));
#904=EDGE_LOOP('',(#2984));
#905=EDGE_LOOP('',(#2985,#2986,#2987,#2988));
#906=EDGE_LOOP('',(#2989));
#907=EDGE_LOOP('',(#2990));
#908=EDGE_LOOP('',(#2991));
#909=EDGE_LOOP('',(#2992));
#910=EDGE_LOOP('',(#2993));
#911=EDGE_LOOP('',(#2994,#2995,#2996,#2997));
#912=EDGE_LOOP('',(#2998,#2999,#3000,#3001));
#913=EDGE_LOOP('',(#3002,#3003,#3004,#3005));
#914=EDGE_LOOP('',(#3006,#3007,#3008,#3009));
#915=EDGE_LOOP('',(#3010,#3011,#3012,#3013));
#916=EDGE_LOOP('',(#3014));
#917=EDGE_LOOP('',(#3015));
#918=EDGE_LOOP('',(#3016,#3017,#3018,#3019));
#919=EDGE_LOOP('',(#3020));
#920=EDGE_LOOP('',(#3021));
#921=EDGE_LOOP('',(#3022,#3023,#3024,#3025));
#922=EDGE_LOOP('',(#3026));
#923=EDGE_LOOP('',(#3027));
#924=EDGE_LOOP('',(#3028,#3029,#3030,#3031));
#925=EDGE_LOOP('',(#3032));
#926=EDGE_LOOP('',(#3033));
#927=EDGE_LOOP('',(#3034,#3035,#3036,#3037));
#928=EDGE_LOOP('',(#3038));
#929=EDGE_LOOP('',(#3039));
#930=EDGE_LOOP('',(#3040,#3041,#3042,#3043));
#931=EDGE_LOOP('',(#3044));
#932=EDGE_LOOP('',(#3045));
#933=EDGE_LOOP('',(#3046,#3047,#3048,#3049));
#934=EDGE_LOOP('',(#3050,#3051,#3052,#3053));
#935=EDGE_LOOP('',(#3054,#3055,#3056,#3057));
#936=EDGE_LOOP('',(#3058,#3059,#3060,#3061));
#937=EDGE_LOOP('',(#3062,#3063,#3064,#3065));
#938=EDGE_LOOP('',(#3066,#3067,#3068,#3069));
#939=EDGE_LOOP('',(#3070));
#940=EDGE_LOOP('',(#3071));
#941=EDGE_LOOP('',(#3072,#3073,#3074,#3075));
#942=EDGE_LOOP('',(#3076,#3077,#3078,#3079));
#943=EDGE_LOOP('',(#3080));
#944=EDGE_LOOP('',(#3081));
#945=EDGE_LOOP('',(#3082,#3083,#3084,#3085));
#946=EDGE_LOOP('',(#3086,#3087,#3088,#3089));
#947=EDGE_LOOP('',(#3090,#3091,#3092,#3093));
#948=EDGE_LOOP('',(#3094,#3095,#3096,#3097));
#949=EDGE_LOOP('',(#3098,#3099,#3100,#3101));
#950=EDGE_LOOP('',(#3102,#3103,#3104,#3105));
#951=EDGE_LOOP('',(#3106,#3107,#3108,#3109));
#952=EDGE_LOOP('',(#3110,#3111,#3112,#3113));
#953=EDGE_LOOP('',(#3114,#3115,#3116,#3117));
#954=EDGE_LOOP('',(#3118,#3119,#3120,#3121));
#955=EDGE_LOOP('',(#3122));
#956=EDGE_LOOP('',(#3123));
#957=EDGE_LOOP('',(#3124));
#958=EDGE_LOOP('',(#3125));
#959=EDGE_LOOP('',(#3126));
#960=EDGE_LOOP('',(#3127));
#961=EDGE_LOOP('',(#3128,#3129,#3130,#3131));
#962=EDGE_LOOP('',(#3132,#3133,#3134,#3135));
#963=EDGE_LOOP('',(#3136));
#964=EDGE_LOOP('',(#3137));
#965=EDGE_LOOP('',(#3138));
#966=EDGE_LOOP('',(#3139));
#967=EDGE_LOOP('',(#3140));
#968=EDGE_LOOP('',(#3141));
#969=EDGE_LOOP('',(#3142,#3143,#3144,#3145));
#970=EDGE_LOOP('',(#3146,#3147,#3148,#3149));
#971=EDGE_LOOP('',(#3150));
#972=EDGE_LOOP('',(#3151,#3152,#3153,#3154));
#973=EDGE_LOOP('',(#3155,#3156,#3157,#3158));
#974=EDGE_LOOP('',(#3159,#3160,#3161,#3162));
#975=EDGE_LOOP('',(#3163));
#976=EDGE_LOOP('',(#3164));
#977=EDGE_LOOP('',(#3165,#3166,#3167,#3168));
#978=EDGE_LOOP('',(#3169,#3170,#3171,#3172));
#979=EDGE_LOOP('',(#3173,#3174,#3175,#3176));
#980=EDGE_LOOP('',(#3177));
#981=EDGE_LOOP('',(#3178,#3179,#3180,#3181));
#982=EDGE_LOOP('',(#3182,#3183,#3184,#3185));
#983=EDGE_LOOP('',(#3186,#3187,#3188,#3189));
#984=EDGE_LOOP('',(#3190,#3191,#3192,#3193));
#985=EDGE_LOOP('',(#3194,#3195,#3196,#3197));
#986=EDGE_LOOP('',(#3198,#3199,#3200,#3201));
#987=EDGE_LOOP('',(#3202,#3203,#3204,#3205,#3206,#3207));
#988=EDGE_LOOP('',(#3208,#3209,#3210,#3211,#3212,#3213));
#989=EDGE_LOOP('',(#3214));
#990=EDGE_LOOP('',(#3215,#3216,#3217,#3218));
#991=EDGE_LOOP('',(#3219,#3220,#3221,#3222));
#992=EDGE_LOOP('',(#3223,#3224,#3225,#3226));
#993=EDGE_LOOP('',(#3227));
#994=EDGE_LOOP('',(#3228));
#995=EDGE_LOOP('',(#3229,#3230,#3231,#3232));
#996=EDGE_LOOP('',(#3233,#3234,#3235,#3236));
#997=EDGE_LOOP('',(#3237,#3238,#3239,#3240));
#998=EDGE_LOOP('',(#3241));
#999=EDGE_LOOP('',(#3242,#3243,#3244,#3245));
#1000=EDGE_LOOP('',(#3246,#3247,#3248,#3249));
#1001=EDGE_LOOP('',(#3250,#3251,#3252,#3253));
#1002=EDGE_LOOP('',(#3254,#3255,#3256,#3257));
#1003=EDGE_LOOP('',(#3258,#3259,#3260,#3261));
#1004=EDGE_LOOP('',(#3262,#3263,#3264,#3265));
#1005=EDGE_LOOP('',(#3266,#3267,#3268,#3269,#3270,#3271));
#1006=EDGE_LOOP('',(#3272,#3273,#3274,#3275,#3276,#3277));
#1007=EDGE_LOOP('',(#3278,#3279,#3280,#3281));
#1008=EDGE_LOOP('',(#3282,#3283,#3284,#3285));
#1009=EDGE_LOOP('',(#3286));
#1010=EDGE_LOOP('',(#3287));
#1011=EDGE_LOOP('',(#3288));
#1012=EDGE_LOOP('',(#3289));
#1013=EDGE_LOOP('',(#3290,#3291,#3292,#3293));
#1014=EDGE_LOOP('',(#3294,#3295,#3296,#3297));
#1015=EDGE_LOOP('',(#3298));
#1016=EDGE_LOOP('',(#3299));
#1017=EDGE_LOOP('',(#3300));
#1018=EDGE_LOOP('',(#3301));
#1019=EDGE_LOOP('',(#3302));
#1020=EDGE_LOOP('',(#3303,#3304,#3305,#3306));
#1021=EDGE_LOOP('',(#3307,#3308,#3309,#3310));
#1022=EDGE_LOOP('',(#3311,#3312,#3313,#3314));
#1023=EDGE_LOOP('',(#3315));
#1024=EDGE_LOOP('',(#3316));
#1025=EDGE_LOOP('',(#3317,#3318,#3319,#3320));
#1026=EDGE_LOOP('',(#3321,#3322,#3323,#3324));
#1027=EDGE_LOOP('',(#3325,#3326,#3327,#3328));
#1028=EDGE_LOOP('',(#3329));
#1029=EDGE_LOOP('',(#3330,#3331,#3332,#3333));
#1030=EDGE_LOOP('',(#3334,#3335,#3336,#3337));
#1031=EDGE_LOOP('',(#3338,#3339,#3340,#3341));
#1032=EDGE_LOOP('',(#3342,#3343,#3344,#3345));
#1033=EDGE_LOOP('',(#3346,#3347,#3348,#3349));
#1034=EDGE_LOOP('',(#3350,#3351,#3352,#3353));
#1035=EDGE_LOOP('',(#3354,#3355,#3356,#3357,#3358,#3359));
#1036=EDGE_LOOP('',(#3360,#3361,#3362,#3363,#3364,#3365));
#1037=LINE('',#5424,#1323);
#1038=LINE('',#5430,#1324);
#1039=LINE('',#5436,#1325);
#1040=LINE('',#5442,#1326);
#1041=LINE('',#5448,#1327);
#1042=LINE('',#5454,#1328);
#1043=LINE('',#5460,#1329);
#1044=LINE('',#5466,#1330);
#1045=LINE('',#5472,#1331);
#1046=LINE('',#5478,#1332);
#1047=LINE('',#5484,#1333);
#1048=LINE('',#5490,#1334);
#1049=LINE('',#5495,#1335);
#1050=LINE('',#5497,#1336);
#1051=LINE('',#5499,#1337);
#1052=LINE('',#5500,#1338);
#1053=LINE('',#5503,#1339);
#1054=LINE('',#5505,#1340);
#1055=LINE('',#5506,#1341);
#1056=LINE('',#5509,#1342);
#1057=LINE('',#5511,#1343);
#1058=LINE('',#5512,#1344);
#1059=LINE('',#5514,#1345);
#1060=LINE('',#5515,#1346);
#1061=LINE('',#5523,#1347);
#1062=LINE('',#5528,#1348);
#1063=LINE('',#5533,#1349);
#1064=LINE('',#5539,#1350);
#1065=LINE('',#5543,#1351);
#1066=LINE('',#5546,#1352);
#1067=LINE('',#5550,#1353);
#1068=LINE('',#5554,#1354);
#1069=LINE('',#5557,#1355);
#1070=LINE('',#5560,#1356);
#1071=LINE('',#5562,#1357);
#1072=LINE('',#5564,#1358);
#1073=LINE('',#5566,#1359);
#1074=LINE('',#5567,#1360);
#1075=LINE('',#5572,#1361);
#1076=LINE('',#5574,#1362);
#1077=LINE('',#5575,#1363);
#1078=LINE('',#5581,#1364);
#1079=LINE('',#5583,#1365);
#1080=LINE('',#5584,#1366);
#1081=LINE('',#5586,#1367);
#1082=LINE('',#5587,#1368);
#1083=LINE('',#5594,#1369);
#1084=LINE('',#5598,#1370);
#1085=LINE('',#5603,#1371);
#1086=LINE('',#5607,#1372);
#1087=LINE('',#5612,#1373);
#1088=LINE('',#5616,#1374);
#1089=LINE('',#5618,#1375);
#1090=LINE('',#5619,#1376);
#1091=LINE('',#5621,#1377);
#1092=LINE('',#5623,#1378);
#1093=LINE('',#5625,#1379);
#1094=LINE('',#5627,#1380);
#1095=LINE('',#5629,#1381);
#1096=LINE('',#5630,#1382);
#1097=LINE('',#5633,#1383);
#1098=LINE('',#5634,#1384);
#1099=LINE('',#5637,#1385);
#1100=LINE('',#5638,#1386);
#1101=LINE('',#5640,#1387);
#1102=LINE('',#5643,#1388);
#1103=LINE('',#5644,#1389);
#1104=LINE('',#5647,#1390);
#1105=LINE('',#5648,#1391);
#1106=LINE('',#5651,#1392);
#1107=LINE('',#5652,#1393);
#1108=LINE('',#5655,#1394);
#1109=LINE('',#5656,#1395);
#1110=LINE('',#5659,#1396);
#1111=LINE('',#5660,#1397);
#1112=LINE('',#5662,#1398);
#1113=LINE('',#5668,#1399);
#1114=LINE('',#5670,#1400);
#1115=LINE('',#5672,#1401);
#1116=LINE('',#5673,#1402);
#1117=LINE('',#5676,#1403);
#1118=LINE('',#5678,#1404);
#1119=LINE('',#5679,#1405);
#1120=LINE('',#5682,#1406);
#1121=LINE('',#5684,#1407);
#1122=LINE('',#5685,#1408);
#1123=LINE('',#5688,#1409);
#1124=LINE('',#5690,#1410);
#1125=LINE('',#5691,#1411);
#1126=LINE('',#5694,#1412);
#1127=LINE('',#5696,#1413);
#1128=LINE('',#5697,#1414);
#1129=LINE('',#5699,#1415);
#1130=LINE('',#5700,#1416);
#1131=LINE('',#5712,#1417);
#1132=LINE('',#5716,#1418);
#1133=LINE('',#5720,#1419);
#1134=LINE('',#5727,#1420);
#1135=LINE('',#5729,#1421);
#1136=LINE('',#5735,#1422);
#1137=LINE('',#5744,#1423);
#1138=LINE('',#5752,#1424);
#1139=LINE('',#5756,#1425);
#1140=LINE('',#5760,#1426);
#1141=LINE('',#5762,#1427);
#1142=LINE('',#5764,#1428);
#1143=LINE('',#5765,#1429);
#1144=LINE('',#5768,#1430);
#1145=LINE('',#5770,#1431);
#1146=LINE('',#5771,#1432);
#1147=LINE('',#5774,#1433);
#1148=LINE('',#5776,#1434);
#1149=LINE('',#5777,#1435);
#1150=LINE('',#5779,#1436);
#1151=LINE('',#5780,#1437);
#1152=LINE('',#5787,#1438);
#1153=LINE('',#5789,#1439);
#1154=LINE('',#5791,#1440);
#1155=LINE('',#5792,#1441);
#1156=LINE('',#5795,#1442);
#1157=LINE('',#5797,#1443);
#1158=LINE('',#5798,#1444);
#1159=LINE('',#5801,#1445);
#1160=LINE('',#5803,#1446);
#1161=LINE('',#5804,#1447);
#1162=LINE('',#5806,#1448);
#1163=LINE('',#5807,#1449);
#1164=LINE('',#5816,#1450);
#1165=LINE('',#5822,#1451);
#1166=LINE('',#5828,#1452);
#1167=LINE('',#5834,#1453);
#1168=LINE('',#5840,#1454);
#1169=LINE('',#5847,#1455);
#1170=LINE('',#5854,#1456);
#1171=LINE('',#5861,#1457);
#1172=LINE('',#5868,#1458);
#1173=LINE('',#5874,#1459);
#1174=LINE('',#5879,#1460);
#1175=LINE('',#5881,#1461);
#1176=LINE('',#5883,#1462);
#1177=LINE('',#5884,#1463);
#1178=LINE('',#5887,#1464);
#1179=LINE('',#5889,#1465);
#1180=LINE('',#5890,#1466);
#1181=LINE('',#5893,#1467);
#1182=LINE('',#5895,#1468);
#1183=LINE('',#5896,#1469);
#1184=LINE('',#5898,#1470);
#1185=LINE('',#5899,#1471);
#1186=LINE('',#5907,#1472);
#1187=LINE('',#5913,#1473);
#1188=LINE('',#5919,#1474);
#1189=LINE('',#5925,#1475);
#1190=LINE('',#5931,#1476);
#1191=LINE('',#5936,#1477);
#1192=LINE('',#5938,#1478);
#1193=LINE('',#5940,#1479);
#1194=LINE('',#5941,#1480);
#1195=LINE('',#5944,#1481);
#1196=LINE('',#5946,#1482);
#1197=LINE('',#5947,#1483);
#1198=LINE('',#5950,#1484);
#1199=LINE('',#5952,#1485);
#1200=LINE('',#5953,#1486);
#1201=LINE('',#5955,#1487);
#1202=LINE('',#5956,#1488);
#1203=LINE('',#5966,#1489);
#1204=LINE('',#5968,#1490);
#1205=LINE('',#5969,#1491);
#1206=LINE('',#5972,#1492);
#1207=LINE('',#5974,#1493);
#1208=LINE('',#5975,#1494);
#1209=LINE('',#5980,#1495);
#1210=LINE('',#5981,#1496);
#1211=LINE('',#5983,#1497);
#1212=LINE('',#5984,#1498);
#1213=LINE('',#5994,#1499);
#1214=LINE('',#6001,#1500);
#1215=LINE('',#6008,#1501);
#1216=LINE('',#6015,#1502);
#1217=LINE('',#6022,#1503);
#1218=LINE('',#6027,#1504);
#1219=LINE('',#6034,#1505);
#1220=LINE('',#6037,#1506);
#1221=LINE('',#6040,#1507);
#1222=LINE('',#6042,#1508);
#1223=LINE('',#6043,#1509);
#1224=LINE('',#6049,#1510);
#1225=LINE('',#6051,#1511);
#1226=LINE('',#6052,#1512);
#1227=LINE('',#6061,#1513);
#1228=LINE('',#6066,#1514);
#1229=LINE('',#6074,#1515);
#1230=LINE('',#6080,#1516);
#1231=LINE('',#6086,#1517);
#1232=LINE('',#6092,#1518);
#1233=LINE('',#6098,#1519);
#1234=LINE('',#6104,#1520);
#1235=LINE('',#6109,#1521);
#1236=LINE('',#6111,#1522);
#1237=LINE('',#6113,#1523);
#1238=LINE('',#6114,#1524);
#1239=LINE('',#6117,#1525);
#1240=LINE('',#6119,#1526);
#1241=LINE('',#6120,#1527);
#1242=LINE('',#6123,#1528);
#1243=LINE('',#6125,#1529);
#1244=LINE('',#6126,#1530);
#1245=LINE('',#6128,#1531);
#1246=LINE('',#6129,#1532);
#1247=LINE('',#6139,#1533);
#1248=LINE('',#6143,#1534);
#1249=LINE('',#6147,#1535);
#1250=LINE('',#6154,#1536);
#1251=LINE('',#6158,#1537);
#1252=LINE('',#6162,#1538);
#1253=LINE('',#6167,#1539);
#1254=LINE('',#6169,#1540);
#1255=LINE('',#6171,#1541);
#1256=LINE('',#6172,#1542);
#1257=LINE('',#6175,#1543);
#1258=LINE('',#6177,#1544);
#1259=LINE('',#6178,#1545);
#1260=LINE('',#6181,#1546);
#1261=LINE('',#6183,#1547);
#1262=LINE('',#6184,#1548);
#1263=LINE('',#6187,#1549);
#1264=LINE('',#6189,#1550);
#1265=LINE('',#6190,#1551);
#1266=LINE('',#6193,#1552);
#1267=LINE('',#6195,#1553);
#1268=LINE('',#6196,#1554);
#1269=LINE('',#6198,#1555);
#1270=LINE('',#6199,#1556);
#1271=LINE('',#6209,#1557);
#1272=LINE('',#6213,#1558);
#1273=LINE('',#6217,#1559);
#1274=LINE('',#6224,#1560);
#1275=LINE('',#6228,#1561);
#1276=LINE('',#6232,#1562);
#1277=LINE('',#6237,#1563);
#1278=LINE('',#6239,#1564);
#1279=LINE('',#6241,#1565);
#1280=LINE('',#6242,#1566);
#1281=LINE('',#6245,#1567);
#1282=LINE('',#6247,#1568);
#1283=LINE('',#6248,#1569);
#1284=LINE('',#6251,#1570);
#1285=LINE('',#6253,#1571);
#1286=LINE('',#6254,#1572);
#1287=LINE('',#6257,#1573);
#1288=LINE('',#6259,#1574);
#1289=LINE('',#6260,#1575);
#1290=LINE('',#6263,#1576);
#1291=LINE('',#6265,#1577);
#1292=LINE('',#6266,#1578);
#1293=LINE('',#6268,#1579);
#1294=LINE('',#6269,#1580);
#1295=LINE('',#6304,#1581);
#1296=LINE('',#6310,#1582);
#1297=LINE('',#6319,#1583);
#1298=LINE('',#6325,#1584);
#1299=LINE('',#6336,#1585);
#1300=LINE('',#6340,#1586);
#1301=LINE('',#6344,#1587);
#1302=LINE('',#6351,#1588);
#1303=LINE('',#6355,#1589);
#1304=LINE('',#6359,#1590);
#1305=LINE('',#6364,#1591);
#1306=LINE('',#6366,#1592);
#1307=LINE('',#6368,#1593);
#1308=LINE('',#6369,#1594);
#1309=LINE('',#6372,#1595);
#1310=LINE('',#6374,#1596);
#1311=LINE('',#6375,#1597);
#1312=LINE('',#6378,#1598);
#1313=LINE('',#6380,#1599);
#1314=LINE('',#6381,#1600);
#1315=LINE('',#6384,#1601);
#1316=LINE('',#6386,#1602);
#1317=LINE('',#6387,#1603);
#1318=LINE('',#6390,#1604);
#1319=LINE('',#6392,#1605);
#1320=LINE('',#6393,#1606);
#1321=LINE('',#6395,#1607);
#1322=LINE('',#6396,#1608);
#1323=VECTOR('',#4277,0.210000000000001);
#1324=VECTOR('',#4284,0.21);
#1325=VECTOR('',#4291,0.21);
#1326=VECTOR('',#4298,0.210000000000001);
#1327=VECTOR('',#4305,0.210000000000001);
#1328=VECTOR('',#4312,0.210000000000001);
#1329=VECTOR('',#4319,0.21);
#1330=VECTOR('',#4326,0.21);
#1331=VECTOR('',#4333,0.21);
#1332=VECTOR('',#4340,0.21);
#1333=VECTOR('',#4347,0.210000000000001);
#1334=VECTOR('',#4354,0.210000000000001);
#1335=VECTOR('',#4359,1.);
#1336=VECTOR('',#4360,1.);
#1337=VECTOR('',#4361,1.);
#1338=VECTOR('',#4362,1.);
#1339=VECTOR('',#4365,1.);
#1340=VECTOR('',#4366,1.);
#1341=VECTOR('',#4367,1.);
#1342=VECTOR('',#4370,1.);
#1343=VECTOR('',#4371,1.);
#1344=VECTOR('',#4372,1.);
#1345=VECTOR('',#4375,1.);
#1346=VECTOR('',#4376,1.);
#1347=VECTOR('',#4387,0.55);
#1348=VECTOR('',#4394,0.6);
#1349=VECTOR('',#4401,0.55);
#1350=VECTOR('',#4408,1.);
#1351=VECTOR('',#4413,1.);
#1352=VECTOR('',#4416,1.);
#1353=VECTOR('',#4419,1.);
#1354=VECTOR('',#4422,1.);
#1355=VECTOR('',#4427,1.);
#1356=VECTOR('',#4430,1.);
#1357=VECTOR('',#4431,1.);
#1358=VECTOR('',#4432,1.);
#1359=VECTOR('',#4433,1.);
#1360=VECTOR('',#4434,1.);
#1361=VECTOR('',#4439,1.);
#1362=VECTOR('',#4440,1.);
#1363=VECTOR('',#4441,1.);
#1364=VECTOR('',#4446,1.);
#1365=VECTOR('',#4447,1.);
#1366=VECTOR('',#4448,1.);
#1367=VECTOR('',#4449,1.);
#1368=VECTOR('',#4450,1.);
#1369=VECTOR('',#4457,0.225);
#1370=VECTOR('',#4462,0.165);
#1371=VECTOR('',#4469,0.275);
#1372=VECTOR('',#4474,0.275);
#1373=VECTOR('',#4479,0.6);
#1374=VECTOR('',#4484,1.);
#1375=VECTOR('',#4485,1.);
#1376=VECTOR('',#4486,1.);
#1377=VECTOR('',#4487,1.);
#1378=VECTOR('',#4488,1.);
#1379=VECTOR('',#4489,1.);
#1380=VECTOR('',#4490,1.);
#1381=VECTOR('',#4491,1.);
#1382=VECTOR('',#4492,1.);
#1383=VECTOR('',#4495,1.);
#1384=VECTOR('',#4496,1.);
#1385=VECTOR('',#4499,1.);
#1386=VECTOR('',#4500,1.);
#1387=VECTOR('',#4503,1.);
#1388=VECTOR('',#4506,1.);
#1389=VECTOR('',#4507,1.);
#1390=VECTOR('',#4510,1.);
#1391=VECTOR('',#4511,1.);
#1392=VECTOR('',#4514,1.);
#1393=VECTOR('',#4515,1.);
#1394=VECTOR('',#4518,1.);
#1395=VECTOR('',#4519,1.);
#1396=VECTOR('',#4522,1.);
#1397=VECTOR('',#4523,1.);
#1398=VECTOR('',#4526,1.);
#1399=VECTOR('',#4533,1.);
#1400=VECTOR('',#4534,1.);
#1401=VECTOR('',#4535,1.);
#1402=VECTOR('',#4536,1.);
#1403=VECTOR('',#4539,1.);
#1404=VECTOR('',#4540,1.);
#1405=VECTOR('',#4541,1.);
#1406=VECTOR('',#4544,1.);
#1407=VECTOR('',#4545,1.);
#1408=VECTOR('',#4546,1.);
#1409=VECTOR('',#4549,1.);
#1410=VECTOR('',#4550,1.);
#1411=VECTOR('',#4551,1.);
#1412=VECTOR('',#4554,1.);
#1413=VECTOR('',#4555,1.);
#1414=VECTOR('',#4556,1.);
#1415=VECTOR('',#4559,1.);
#1416=VECTOR('',#4560,1.);
#1417=VECTOR('',#4577,0.4);
#1418=VECTOR('',#4582,0.425);
#1419=VECTOR('',#4587,0.41);
#1420=VECTOR('',#4596,0.26);
#1421=VECTOR('',#4599,0.25);
#1422=VECTOR('',#4606,0.475);
#1423=VECTOR('',#4617,0.475);
#1424=VECTOR('',#4628,0.275);
#1425=VECTOR('',#4633,0.275);
#1426=VECTOR('',#4636,1.);
#1427=VECTOR('',#4637,1.);
#1428=VECTOR('',#4638,1.);
#1429=VECTOR('',#4639,1.);
#1430=VECTOR('',#4642,1.);
#1431=VECTOR('',#4643,1.);
#1432=VECTOR('',#4644,1.);
#1433=VECTOR('',#4647,1.);
#1434=VECTOR('',#4648,1.);
#1435=VECTOR('',#4649,1.);
#1436=VECTOR('',#4652,1.);
#1437=VECTOR('',#4653,1.);
#1438=VECTOR('',#4662,1.);
#1439=VECTOR('',#4663,1.);
#1440=VECTOR('',#4664,1.);
#1441=VECTOR('',#4665,1.);
#1442=VECTOR('',#4668,1.);
#1443=VECTOR('',#4669,1.);
#1444=VECTOR('',#4670,1.);
#1445=VECTOR('',#4673,1.);
#1446=VECTOR('',#4674,1.);
#1447=VECTOR('',#4675,1.);
#1448=VECTOR('',#4678,1.);
#1449=VECTOR('',#4679,1.);
#1450=VECTOR('',#4692,0.165);
#1451=VECTOR('',#4699,0.165);
#1452=VECTOR('',#4706,0.165);
#1453=VECTOR('',#4713,0.165);
#1454=VECTOR('',#4720,0.210000000000001);
#1455=VECTOR('',#4729,0.210000000000001);
#1456=VECTOR('',#4738,0.210000000000001);
#1457=VECTOR('',#4747,0.210000000000001);
#1458=VECTOR('',#4756,1.05);
#1459=VECTOR('',#4763,1.05);
#1460=VECTOR('',#4768,1.);
#1461=VECTOR('',#4769,1.);
#1462=VECTOR('',#4770,1.);
#1463=VECTOR('',#4771,1.);
#1464=VECTOR('',#4774,1.);
#1465=VECTOR('',#4775,1.);
#1466=VECTOR('',#4776,1.);
#1467=VECTOR('',#4779,1.);
#1468=VECTOR('',#4780,1.);
#1469=VECTOR('',#4781,1.);
#1470=VECTOR('',#4784,1.);
#1471=VECTOR('',#4785,1.);
#1472=VECTOR('',#4796,0.25);
#1473=VECTOR('',#4803,0.274999999999999);
#1474=VECTOR('',#4810,0.275);
#1475=VECTOR('',#4817,0.275);
#1476=VECTOR('',#4824,0.274999999999999);
#1477=VECTOR('',#4829,1.);
#1478=VECTOR('',#4830,1.);
#1479=VECTOR('',#4831,1.);
#1480=VECTOR('',#4832,1.);
#1481=VECTOR('',#4835,1.);
#1482=VECTOR('',#4836,1.);
#1483=VECTOR('',#4837,1.);
#1484=VECTOR('',#4840,1.);
#1485=VECTOR('',#4841,1.);
#1486=VECTOR('',#4842,1.);
#1487=VECTOR('',#4845,1.);
#1488=VECTOR('',#4846,1.);
#1489=VECTOR('',#4859,1.);
#1490=VECTOR('',#4860,1.);
#1491=VECTOR('',#4861,1.);
#1492=VECTOR('',#4864,1.);
#1493=VECTOR('',#4865,1.);
#1494=VECTOR('',#4866,1.);
#1495=VECTOR('',#4871,1.);
#1496=VECTOR('',#4872,1.);
#1497=VECTOR('',#4875,1.);
#1498=VECTOR('',#4876,1.);
#1499=VECTOR('',#4889,1.05);
#1500=VECTOR('',#4898,1.);
#1501=VECTOR('',#4907,1.05);
#1502=VECTOR('',#4916,1.);
#1503=VECTOR('',#4925,1.05);
#1504=VECTOR('',#4932,0.9);
#1505=VECTOR('',#4939,1.);
#1506=VECTOR('',#4942,1.);
#1507=VECTOR('',#4945,1.);
#1508=VECTOR('',#4946,1.);
#1509=VECTOR('',#4947,1.);
#1510=VECTOR('',#4954,1.);
#1511=VECTOR('',#4957,1.);
#1512=VECTOR('',#4958,1.);
#1513=VECTOR('',#4969,0.895);
#1514=VECTOR('',#4976,0.605);
#1515=VECTOR('',#4987,0.225);
#1516=VECTOR('',#4994,0.225);
#1517=VECTOR('',#5001,0.225);
#1518=VECTOR('',#5008,0.225);
#1519=VECTOR('',#5015,0.7);
#1520=VECTOR('',#5022,0.7);
#1521=VECTOR('',#5027,1.);
#1522=VECTOR('',#5028,1.);
#1523=VECTOR('',#5029,1.);
#1524=VECTOR('',#5030,1.);
#1525=VECTOR('',#5033,1.);
#1526=VECTOR('',#5034,1.);
#1527=VECTOR('',#5035,1.);
#1528=VECTOR('',#5038,1.);
#1529=VECTOR('',#5039,1.);
#1530=VECTOR('',#5040,1.);
#1531=VECTOR('',#5043,1.);
#1532=VECTOR('',#5044,1.);
#1533=VECTOR('',#5059,0.325);
#1534=VECTOR('',#5064,0.35);
#1535=VECTOR('',#5069,0.335);
#1536=VECTOR('',#5078,0.21);
#1537=VECTOR('',#5083,0.2);
#1538=VECTOR('',#5088,0.18);
#1539=VECTOR('',#5093,1.);
#1540=VECTOR('',#5094,1.);
#1541=VECTOR('',#5095,1.);
#1542=VECTOR('',#5096,1.);
#1543=VECTOR('',#5099,1.);
#1544=VECTOR('',#5100,1.);
#1545=VECTOR('',#5101,1.);
#1546=VECTOR('',#5104,1.);
#1547=VECTOR('',#5105,1.);
#1548=VECTOR('',#5106,1.);
#1549=VECTOR('',#5109,1.);
#1550=VECTOR('',#5110,1.);
#1551=VECTOR('',#5111,1.);
#1552=VECTOR('',#5114,1.);
#1553=VECTOR('',#5115,1.);
#1554=VECTOR('',#5116,1.);
#1555=VECTOR('',#5119,1.);
#1556=VECTOR('',#5120,1.);
#1557=VECTOR('',#5135,0.4);
#1558=VECTOR('',#5140,0.425);
#1559=VECTOR('',#5145,0.41);
#1560=VECTOR('',#5154,0.26);
#1561=VECTOR('',#5159,0.25);
#1562=VECTOR('',#5164,0.225);
#1563=VECTOR('',#5169,1.);
#1564=VECTOR('',#5170,1.);
#1565=VECTOR('',#5171,1.);
#1566=VECTOR('',#5172,1.);
#1567=VECTOR('',#5175,1.);
#1568=VECTOR('',#5176,1.);
#1569=VECTOR('',#5177,1.);
#1570=VECTOR('',#5180,1.);
#1571=VECTOR('',#5181,1.);
#1572=VECTOR('',#5182,1.);
#1573=VECTOR('',#5185,1.);
#1574=VECTOR('',#5186,1.);
#1575=VECTOR('',#5187,1.);
#1576=VECTOR('',#5190,1.);
#1577=VECTOR('',#5191,1.);
#1578=VECTOR('',#5192,1.);
#1579=VECTOR('',#5195,1.);
#1580=VECTOR('',#5196,1.);
#1581=VECTOR('',#5261,0.33);
#1582=VECTOR('',#5268,1.5);
#1583=VECTOR('',#5281,0.32);
#1584=VECTOR('',#5288,0.6);
#1585=VECTOR('',#5305,0.475);
#1586=VECTOR('',#5310,0.5);
#1587=VECTOR('',#5315,0.485);
#1588=VECTOR('',#5324,0.31);
#1589=VECTOR('',#5329,0.3);
#1590=VECTOR('',#5334,0.27);
#1591=VECTOR('',#5339,1.);
#1592=VECTOR('',#5340,1.);
#1593=VECTOR('',#5341,1.);
#1594=VECTOR('',#5342,1.);
#1595=VECTOR('',#5345,1.);
#1596=VECTOR('',#5346,1.);
#1597=VECTOR('',#5347,1.);
#1598=VECTOR('',#5350,1.);
#1599=VECTOR('',#5351,1.);
#1600=VECTOR('',#5352,1.);
#1601=VECTOR('',#5355,1.);
#1602=VECTOR('',#5356,1.);
#1603=VECTOR('',#5357,1.);
#1604=VECTOR('',#5360,1.);
#1605=VECTOR('',#5361,1.);
#1606=VECTOR('',#5362,1.);
#1607=VECTOR('',#5365,1.);
#1608=VECTOR('',#5366,1.);
#1609=CIRCLE('',#3839,0.210000000000001);
#1610=CIRCLE('',#3840,0.210000000000001);
#1611=CIRCLE('',#3842,0.21);
#1612=CIRCLE('',#3843,0.21);
#1613=CIRCLE('',#3845,0.21);
#1614=CIRCLE('',#3846,0.21);
#1615=CIRCLE('',#3848,0.210000000000001);
#1616=CIRCLE('',#3849,0.210000000000001);
#1617=CIRCLE('',#3851,0.210000000000001);
#1618=CIRCLE('',#3852,0.210000000000001);
#1619=CIRCLE('',#3854,0.210000000000001);
#1620=CIRCLE('',#3855,0.210000000000001);
#1621=CIRCLE('',#3857,0.21);
#1622=CIRCLE('',#3858,0.21);
#1623=CIRCLE('',#3860,0.21);
#1624=CIRCLE('',#3861,0.21);
#1625=CIRCLE('',#3863,0.21);
#1626=CIRCLE('',#3864,0.21);
#1627=CIRCLE('',#3866,0.21);
#1628=CIRCLE('',#3867,0.21);
#1629=CIRCLE('',#3869,0.210000000000001);
#1630=CIRCLE('',#3870,0.210000000000001);
#1631=CIRCLE('',#3872,0.210000000000001);
#1632=CIRCLE('',#3873,0.210000000000001);
#1633=CIRCLE('',#3882,0.6);
#1634=CIRCLE('',#3883,0.5);
#1635=CIRCLE('',#3885,0.6);
#1636=CIRCLE('',#3888,0.5);
#1637=CIRCLE('',#3892,0.525);
#1638=CIRCLE('',#3894,0.525);
#1639=CIRCLE('',#3896,0.525);
#1640=CIRCLE('',#3897,0.525);
#1641=CIRCLE('',#3900,0.275);
#1642=CIRCLE('',#3902,0.165);
#1643=CIRCLE('',#3904,0.275);
#1644=CIRCLE('',#3906,0.225);
#1645=CIRCLE('',#3907,0.225);
#1646=CIRCLE('',#3909,0.165);
#1647=CIRCLE('',#3911,0.275);
#1648=CIRCLE('',#3913,0.275);
#1649=CIRCLE('',#3915,0.6);
#1650=CIRCLE('',#3916,0.6);
#1651=CIRCLE('',#3938,0.24505);
#1652=CIRCLE('',#3940,0.375);
#1653=CIRCLE('',#3942,0.425);
#1654=CIRCLE('',#3944,0.425);
#1655=CIRCLE('',#3946,0.395);
#1656=CIRCLE('',#3948,0.27);
#1657=CIRCLE('',#3950,0.24505);
#1658=CIRCLE('',#3954,0.475);
#1659=CIRCLE('',#3955,0.475);
#1660=CIRCLE('',#3957,0.275);
#1661=CIRCLE('',#3959,0.475);
#1662=CIRCLE('',#3960,0.475);
#1663=CIRCLE('',#3962,0.275);
#1664=CIRCLE('',#3964,0.275);
#1665=CIRCLE('',#3966,0.275);
#1666=CIRCLE('',#3983,0.165);
#1667=CIRCLE('',#3984,0.165);
#1668=CIRCLE('',#3986,0.165);
#1669=CIRCLE('',#3987,0.165);
#1670=CIRCLE('',#3989,0.165);
#1671=CIRCLE('',#3990,0.165);
#1672=CIRCLE('',#3992,0.165);
#1673=CIRCLE('',#3993,0.165);
#1674=CIRCLE('',#3995,0.210000000000001);
#1675=CIRCLE('',#3996,0.210000000000001);
#1676=CIRCLE('',#3999,0.210000000000001);
#1677=CIRCLE('',#4000,0.210000000000001);
#1678=CIRCLE('',#4003,0.210000000000001);
#1679=CIRCLE('',#4004,0.210000000000001);
#1680=CIRCLE('',#4007,0.210000000000001);
#1681=CIRCLE('',#4008,0.210000000000001);
#1682=CIRCLE('',#4011,1.05);
#1683=CIRCLE('',#4012,1.05);
#1684=CIRCLE('',#4014,1.05);
#1685=CIRCLE('',#4015,1.05);
#1686=CIRCLE('',#4024,0.25);
#1687=CIRCLE('',#4025,0.25);
#1688=CIRCLE('',#4027,0.274999999999999);
#1689=CIRCLE('',#4028,0.274999999999999);
#1690=CIRCLE('',#4030,0.275);
#1691=CIRCLE('',#4031,0.275);
#1692=CIRCLE('',#4033,0.275);
#1693=CIRCLE('',#4034,0.275);
#1694=CIRCLE('',#4036,0.274999999999999);
#1695=CIRCLE('',#4037,0.274999999999999);
#1696=CIRCLE('',#4047,0.9);
#1697=CIRCLE('',#4050,0.9);
#1698=CIRCLE('',#4054,1.05);
#1699=CIRCLE('',#4055,0.9);
#1700=CIRCLE('',#4057,1.05);
#1701=CIRCLE('',#4059,1.);
#1702=CIRCLE('',#4061,1.);
#1703=CIRCLE('',#4063,1.05);
#1704=CIRCLE('',#4065,1.05);
#1705=CIRCLE('',#4067,1.);
#1706=CIRCLE('',#4069,1.);
#1707=CIRCLE('',#4071,1.05);
#1708=CIRCLE('',#4073,1.05);
#1709=CIRCLE('',#4075,0.9);
#1710=CIRCLE('',#4079,0.895);
#1711=CIRCLE('',#4080,0.605);
#1712=CIRCLE('',#4083,0.895);
#1713=CIRCLE('',#4084,0.605);
#1714=CIRCLE('',#4087,0.895);
#1715=CIRCLE('',#4088,0.605);
#1716=CIRCLE('',#4090,0.895);
#1717=CIRCLE('',#4092,0.605);
#1718=CIRCLE('',#4098,0.225);
#1719=CIRCLE('',#4099,0.225);
#1720=CIRCLE('',#4101,0.225);
#1721=CIRCLE('',#4102,0.225);
#1722=CIRCLE('',#4104,0.225);
#1723=CIRCLE('',#4105,0.225);
#1724=CIRCLE('',#4107,0.225);
#1725=CIRCLE('',#4108,0.225);
#1726=CIRCLE('',#4110,0.7);
#1727=CIRCLE('',#4111,0.7);
#1728=CIRCLE('',#4113,0.7);
#1729=CIRCLE('',#4114,0.7);
#1730=CIRCLE('',#4123,0.3);
#1731=CIRCLE('',#4125,0.35);
#1732=CIRCLE('',#4127,0.35);
#1733=CIRCLE('',#4129,0.32);
#1734=CIRCLE('',#4131,0.22);
#1735=CIRCLE('',#4133,0.1954);
#1736=CIRCLE('',#4135,0.1954);
#1737=CIRCLE('',#4137,0.16);
#1738=CIRCLE('',#4149,0.375);
#1739=CIRCLE('',#4151,0.425);
#1740=CIRCLE('',#4153,0.425);
#1741=CIRCLE('',#4155,0.395);
#1742=CIRCLE('',#4157,0.27);
#1743=CIRCLE('',#4159,0.24505);
#1744=CIRCLE('',#4161,0.24505);
#1745=CIRCLE('',#4163,0.2);
#1746=CIRCLE('',#4202,0.33);
#1747=CIRCLE('',#4203,0.33);
#1748=CIRCLE('',#4205,1.5);
#1749=CIRCLE('',#4206,1.5);
#1750=CIRCLE('',#4211,0.32);
#1751=CIRCLE('',#4212,0.32);
#1752=CIRCLE('',#4214,0.6);
#1753=CIRCLE('',#4215,0.6);
#1754=CIRCLE('',#4220,0.45);
#1755=CIRCLE('',#4222,0.5);
#1756=CIRCLE('',#4224,0.5);
#1757=CIRCLE('',#4226,0.47);
#1758=CIRCLE('',#4228,0.32);
#1759=CIRCLE('',#4230,0.2942);
#1760=CIRCLE('',#4232,0.2942);
#1761=CIRCLE('',#4234,0.24);
#1762=VERTEX_POINT('',#5421);
#1763=VERTEX_POINT('',#5423);
#1764=VERTEX_POINT('',#5427);
#1765=VERTEX_POINT('',#5429);
#1766=VERTEX_POINT('',#5433);
#1767=VERTEX_POINT('',#5435);
#1768=VERTEX_POINT('',#5439);
#1769=VERTEX_POINT('',#5441);
#1770=VERTEX_POINT('',#5445);
#1771=VERTEX_POINT('',#5447);
#1772=VERTEX_POINT('',#5451);
#1773=VERTEX_POINT('',#5453);
#1774=VERTEX_POINT('',#5457);
#1775=VERTEX_POINT('',#5459);
#1776=VERTEX_POINT('',#5463);
#1777=VERTEX_POINT('',#5465);
#1778=VERTEX_POINT('',#5469);
#1779=VERTEX_POINT('',#5471);
#1780=VERTEX_POINT('',#5475);
#1781=VERTEX_POINT('',#5477);
#1782=VERTEX_POINT('',#5481);
#1783=VERTEX_POINT('',#5483);
#1784=VERTEX_POINT('',#5487);
#1785=VERTEX_POINT('',#5489);
#1786=VERTEX_POINT('',#5493);
#1787=VERTEX_POINT('',#5494);
#1788=VERTEX_POINT('',#5496);
#1789=VERTEX_POINT('',#5498);
#1790=VERTEX_POINT('',#5502);
#1791=VERTEX_POINT('',#5504);
#1792=VERTEX_POINT('',#5508);
#1793=VERTEX_POINT('',#5510);
#1794=VERTEX_POINT('',#5520);
#1795=VERTEX_POINT('',#5522);
#1796=VERTEX_POINT('',#5526);
#1797=VERTEX_POINT('',#5531);
#1798=VERTEX_POINT('',#5537);
#1799=VERTEX_POINT('',#5538);
#1800=VERTEX_POINT('',#5542);
#1801=VERTEX_POINT('',#5544);
#1802=VERTEX_POINT('',#5548);
#1803=VERTEX_POINT('',#5549);
#1804=VERTEX_POINT('',#5551);
#1805=VERTEX_POINT('',#5553);
#1806=VERTEX_POINT('',#5559);
#1807=VERTEX_POINT('',#5561);
#1808=VERTEX_POINT('',#5563);
#1809=VERTEX_POINT('',#5565);
#1810=VERTEX_POINT('',#5568);
#1811=VERTEX_POINT('',#5571);
#1812=VERTEX_POINT('',#5573);
#1813=VERTEX_POINT('',#5576);
#1814=VERTEX_POINT('',#5579);
#1815=VERTEX_POINT('',#5580);
#1816=VERTEX_POINT('',#5582);
#1817=VERTEX_POINT('',#5585);
#1818=VERTEX_POINT('',#5588);
#1819=VERTEX_POINT('',#5591);
#1820=VERTEX_POINT('',#5593);
#1821=VERTEX_POINT('',#5597);
#1822=VERTEX_POINT('',#5601);
#1823=VERTEX_POINT('',#5605);
#1824=VERTEX_POINT('',#5609);
#1825=VERTEX_POINT('',#5611);
#1826=VERTEX_POINT('',#5615);
#1827=VERTEX_POINT('',#5617);
#1828=VERTEX_POINT('',#5620);
#1829=VERTEX_POINT('',#5622);
#1830=VERTEX_POINT('',#5624);
#1831=VERTEX_POINT('',#5626);
#1832=VERTEX_POINT('',#5628);
#1833=VERTEX_POINT('',#5632);
#1834=VERTEX_POINT('',#5636);
#1835=VERTEX_POINT('',#5642);
#1836=VERTEX_POINT('',#5646);
#1837=VERTEX_POINT('',#5650);
#1838=VERTEX_POINT('',#5654);
#1839=VERTEX_POINT('',#5658);
#1840=VERTEX_POINT('',#5666);
#1841=VERTEX_POINT('',#5667);
#1842=VERTEX_POINT('',#5669);
#1843=VERTEX_POINT('',#5671);
#1844=VERTEX_POINT('',#5675);
#1845=VERTEX_POINT('',#5677);
#1846=VERTEX_POINT('',#5681);
#1847=VERTEX_POINT('',#5683);
#1848=VERTEX_POINT('',#5687);
#1849=VERTEX_POINT('',#5689);
#1850=VERTEX_POINT('',#5693);
#1851=VERTEX_POINT('',#5695);
#1852=VERTEX_POINT('',#5704);
#1853=VERTEX_POINT('',#5707);
#1854=VERTEX_POINT('',#5710);
#1855=VERTEX_POINT('',#5714);
#1856=VERTEX_POINT('',#5718);
#1857=VERTEX_POINT('',#5722);
#1858=VERTEX_POINT('',#5725);
#1859=VERTEX_POINT('',#5732);
#1860=VERTEX_POINT('',#5734);
#1861=VERTEX_POINT('',#5738);
#1862=VERTEX_POINT('',#5741);
#1863=VERTEX_POINT('',#5743);
#1864=VERTEX_POINT('',#5747);
#1865=VERTEX_POINT('',#5750);
#1866=VERTEX_POINT('',#5754);
#1867=VERTEX_POINT('',#5758);
#1868=VERTEX_POINT('',#5759);
#1869=VERTEX_POINT('',#5761);
#1870=VERTEX_POINT('',#5763);
#1871=VERTEX_POINT('',#5767);
#1872=VERTEX_POINT('',#5769);
#1873=VERTEX_POINT('',#5773);
#1874=VERTEX_POINT('',#5775);
#1875=VERTEX_POINT('',#5785);
#1876=VERTEX_POINT('',#5786);
#1877=VERTEX_POINT('',#5788);
#1878=VERTEX_POINT('',#5790);
#1879=VERTEX_POINT('',#5794);
#1880=VERTEX_POINT('',#5796);
#1881=VERTEX_POINT('',#5800);
#1882=VERTEX_POINT('',#5802);
#1883=VERTEX_POINT('',#5813);
#1884=VERTEX_POINT('',#5815);
#1885=VERTEX_POINT('',#5819);
#1886=VERTEX_POINT('',#5821);
#1887=VERTEX_POINT('',#5825);
#1888=VERTEX_POINT('',#5827);
#1889=VERTEX_POINT('',#5831);
#1890=VERTEX_POINT('',#5833);
#1891=VERTEX_POINT('',#5837);
#1892=VERTEX_POINT('',#5839);
#1893=VERTEX_POINT('',#5844);
#1894=VERTEX_POINT('',#5846);
#1895=VERTEX_POINT('',#5851);
#1896=VERTEX_POINT('',#5853);
#1897=VERTEX_POINT('',#5858);
#1898=VERTEX_POINT('',#5860);
#1899=VERTEX_POINT('',#5865);
#1900=VERTEX_POINT('',#5867);
#1901=VERTEX_POINT('',#5871);
#1902=VERTEX_POINT('',#5873);
#1903=VERTEX_POINT('',#5877);
#1904=VERTEX_POINT('',#5878);
#1905=VERTEX_POINT('',#5880);
#1906=VERTEX_POINT('',#5882);
#1907=VERTEX_POINT('',#5886);
#1908=VERTEX_POINT('',#5888);
#1909=VERTEX_POINT('',#5892);
#1910=VERTEX_POINT('',#5894);
#1911=VERTEX_POINT('',#5904);
#1912=VERTEX_POINT('',#5906);
#1913=VERTEX_POINT('',#5910);
#1914=VERTEX_POINT('',#5912);
#1915=VERTEX_POINT('',#5916);
#1916=VERTEX_POINT('',#5918);
#1917=VERTEX_POINT('',#5922);
#1918=VERTEX_POINT('',#5924);
#1919=VERTEX_POINT('',#5928);
#1920=VERTEX_POINT('',#5930);
#1921=VERTEX_POINT('',#5934);
#1922=VERTEX_POINT('',#5935);
#1923=VERTEX_POINT('',#5937);
#1924=VERTEX_POINT('',#5939);
#1925=VERTEX_POINT('',#5943);
#1926=VERTEX_POINT('',#5945);
#1927=VERTEX_POINT('',#5949);
#1928=VERTEX_POINT('',#5951);
#1929=VERTEX_POINT('',#5962);
#1930=VERTEX_POINT('',#5963);
#1931=VERTEX_POINT('',#5965);
#1932=VERTEX_POINT('',#5967);
#1933=VERTEX_POINT('',#5971);
#1934=VERTEX_POINT('',#5973);
#1935=VERTEX_POINT('',#5977);
#1936=VERTEX_POINT('',#5979);
#1937=VERTEX_POINT('',#5987);
#1938=VERTEX_POINT('',#5989);
#1939=VERTEX_POINT('',#5992);
#1940=VERTEX_POINT('',#5996);
#1941=VERTEX_POINT('',#5999);
#1942=VERTEX_POINT('',#6003);
#1943=VERTEX_POINT('',#6006);
#1944=VERTEX_POINT('',#6010);
#1945=VERTEX_POINT('',#6013);
#1946=VERTEX_POINT('',#6017);
#1947=VERTEX_POINT('',#6020);
#1948=VERTEX_POINT('',#6024);
#1949=VERTEX_POINT('',#6030);
#1950=VERTEX_POINT('',#6031);
#1951=VERTEX_POINT('',#6033);
#1952=VERTEX_POINT('',#6035);
#1953=VERTEX_POINT('',#6039);
#1954=VERTEX_POINT('',#6041);
#1955=VERTEX_POINT('',#6045);
#1956=VERTEX_POINT('',#6047);
#1957=VERTEX_POINT('',#6054);
#1958=VERTEX_POINT('',#6056);
#1959=VERTEX_POINT('',#6059);
#1960=VERTEX_POINT('',#6063);
#1961=VERTEX_POINT('',#6071);
#1962=VERTEX_POINT('',#6073);
#1963=VERTEX_POINT('',#6077);
#1964=VERTEX_POINT('',#6079);
#1965=VERTEX_POINT('',#6083);
#1966=VERTEX_POINT('',#6085);
#1967=VERTEX_POINT('',#6089);
#1968=VERTEX_POINT('',#6091);
#1969=VERTEX_POINT('',#6095);
#1970=VERTEX_POINT('',#6097);
#1971=VERTEX_POINT('',#6101);
#1972=VERTEX_POINT('',#6103);
#1973=VERTEX_POINT('',#6107);
#1974=VERTEX_POINT('',#6108);
#1975=VERTEX_POINT('',#6110);
#1976=VERTEX_POINT('',#6112);
#1977=VERTEX_POINT('',#6116);
#1978=VERTEX_POINT('',#6118);
#1979=VERTEX_POINT('',#6122);
#1980=VERTEX_POINT('',#6124);
#1981=VERTEX_POINT('',#6134);
#1982=VERTEX_POINT('',#6137);
#1983=VERTEX_POINT('',#6141);
#1984=VERTEX_POINT('',#6145);
#1985=VERTEX_POINT('',#6149);
#1986=VERTEX_POINT('',#6152);
#1987=VERTEX_POINT('',#6156);
#1988=VERTEX_POINT('',#6160);
#1989=VERTEX_POINT('',#6165);
#1990=VERTEX_POINT('',#6166);
#1991=VERTEX_POINT('',#6168);
#1992=VERTEX_POINT('',#6170);
#1993=VERTEX_POINT('',#6174);
#1994=VERTEX_POINT('',#6176);
#1995=VERTEX_POINT('',#6180);
#1996=VERTEX_POINT('',#6182);
#1997=VERTEX_POINT('',#6186);
#1998=VERTEX_POINT('',#6188);
#1999=VERTEX_POINT('',#6192);
#2000=VERTEX_POINT('',#6194);
#2001=VERTEX_POINT('',#6204);
#2002=VERTEX_POINT('',#6207);
#2003=VERTEX_POINT('',#6211);
#2004=VERTEX_POINT('',#6215);
#2005=VERTEX_POINT('',#6219);
#2006=VERTEX_POINT('',#6222);
#2007=VERTEX_POINT('',#6226);
#2008=VERTEX_POINT('',#6230);
#2009=VERTEX_POINT('',#6235);
#2010=VERTEX_POINT('',#6236);
#2011=VERTEX_POINT('',#6238);
#2012=VERTEX_POINT('',#6240);
#2013=VERTEX_POINT('',#6244);
#2014=VERTEX_POINT('',#6246);
#2015=VERTEX_POINT('',#6250);
#2016=VERTEX_POINT('',#6252);
#2017=VERTEX_POINT('',#6256);
#2018=VERTEX_POINT('',#6258);
#2019=VERTEX_POINT('',#6262);
#2020=VERTEX_POINT('',#6264);
#2021=VERTEX_POINT('',#6301);
#2022=VERTEX_POINT('',#6303);
#2023=VERTEX_POINT('',#6307);
#2024=VERTEX_POINT('',#6309);
#2025=VERTEX_POINT('',#6316);
#2026=VERTEX_POINT('',#6318);
#2027=VERTEX_POINT('',#6322);
#2028=VERTEX_POINT('',#6324);
#2029=VERTEX_POINT('',#6331);
#2030=VERTEX_POINT('',#6334);
#2031=VERTEX_POINT('',#6338);
#2032=VERTEX_POINT('',#6342);
#2033=VERTEX_POINT('',#6346);
#2034=VERTEX_POINT('',#6349);
#2035=VERTEX_POINT('',#6353);
#2036=VERTEX_POINT('',#6357);
#2037=VERTEX_POINT('',#6362);
#2038=VERTEX_POINT('',#6363);
#2039=VERTEX_POINT('',#6365);
#2040=VERTEX_POINT('',#6367);
#2041=VERTEX_POINT('',#6371);
#2042=VERTEX_POINT('',#6373);
#2043=VERTEX_POINT('',#6377);
#2044=VERTEX_POINT('',#6379);
#2045=VERTEX_POINT('',#6383);
#2046=VERTEX_POINT('',#6385);
#2047=VERTEX_POINT('',#6389);
#2048=VERTEX_POINT('',#6391);
#2049=EDGE_CURVE('',#1762,#1762,#1609,.T.);
#2050=EDGE_CURVE('',#1762,#1763,#1037,.T.);
#2051=EDGE_CURVE('',#1763,#1763,#1610,.T.);
#2052=EDGE_CURVE('',#1764,#1764,#1611,.T.);
#2053=EDGE_CURVE('',#1764,#1765,#1038,.T.);
#2054=EDGE_CURVE('',#1765,#1765,#1612,.T.);
#2055=EDGE_CURVE('',#1766,#1766,#1613,.T.);
#2056=EDGE_CURVE('',#1766,#1767,#1039,.T.);
#2057=EDGE_CURVE('',#1767,#1767,#1614,.T.);
#2058=EDGE_CURVE('',#1768,#1768,#1615,.T.);
#2059=EDGE_CURVE('',#1768,#1769,#1040,.T.);
#2060=EDGE_CURVE('',#1769,#1769,#1616,.T.);
#2061=EDGE_CURVE('',#1770,#1770,#1617,.T.);
#2062=EDGE_CURVE('',#1770,#1771,#1041,.T.);
#2063=EDGE_CURVE('',#1771,#1771,#1618,.T.);
#2064=EDGE_CURVE('',#1772,#1772,#1619,.T.);
#2065=EDGE_CURVE('',#1772,#1773,#1042,.T.);
#2066=EDGE_CURVE('',#1773,#1773,#1620,.T.);
#2067=EDGE_CURVE('',#1774,#1774,#1621,.T.);
#2068=EDGE_CURVE('',#1774,#1775,#1043,.T.);
#2069=EDGE_CURVE('',#1775,#1775,#1622,.T.);
#2070=EDGE_CURVE('',#1776,#1776,#1623,.T.);
#2071=EDGE_CURVE('',#1776,#1777,#1044,.T.);
#2072=EDGE_CURVE('',#1777,#1777,#1624,.T.);
#2073=EDGE_CURVE('',#1778,#1778,#1625,.T.);
#2074=EDGE_CURVE('',#1778,#1779,#1045,.T.);
#2075=EDGE_CURVE('',#1779,#1779,#1626,.T.);
#2076=EDGE_CURVE('',#1780,#1780,#1627,.T.);
#2077=EDGE_CURVE('',#1780,#1781,#1046,.T.);
#2078=EDGE_CURVE('',#1781,#1781,#1628,.T.);
#2079=EDGE_CURVE('',#1782,#1782,#1629,.T.);
#2080=EDGE_CURVE('',#1782,#1783,#1047,.T.);
#2081=EDGE_CURVE('',#1783,#1783,#1630,.T.);
#2082=EDGE_CURVE('',#1784,#1784,#1631,.T.);
#2083=EDGE_CURVE('',#1784,#1785,#1048,.T.);
#2084=EDGE_CURVE('',#1785,#1785,#1632,.T.);
#2085=EDGE_CURVE('',#1786,#1787,#1049,.T.);
#2086=EDGE_CURVE('',#1787,#1788,#1050,.T.);
#2087=EDGE_CURVE('',#1789,#1788,#1051,.T.);
#2088=EDGE_CURVE('',#1786,#1789,#1052,.T.);
#2089=EDGE_CURVE('',#1790,#1786,#1053,.T.);
#2090=EDGE_CURVE('',#1791,#1789,#1054,.T.);
#2091=EDGE_CURVE('',#1790,#1791,#1055,.T.);
#2092=EDGE_CURVE('',#1792,#1790,#1056,.T.);
#2093=EDGE_CURVE('',#1793,#1791,#1057,.T.);
#2094=EDGE_CURVE('',#1792,#1793,#1058,.T.);
#2095=EDGE_CURVE('',#1787,#1792,#1059,.T.);
#2096=EDGE_CURVE('',#1788,#1793,#1060,.T.);
#2097=EDGE_CURVE('',#1794,#1794,#1633,.T.);
#2098=EDGE_CURVE('',#1794,#1795,#1061,.T.);
#2099=EDGE_CURVE('',#1795,#1795,#1634,.T.);
#2100=EDGE_CURVE('',#1796,#1796,#1635,.T.);
#2101=EDGE_CURVE('',#1796,#1794,#1062,.T.);
#2102=EDGE_CURVE('',#1797,#1797,#1636,.T.);
#2103=EDGE_CURVE('',#1797,#1796,#1063,.T.);
#2104=EDGE_CURVE('',#1798,#1799,#1064,.T.);
#2105=EDGE_CURVE('',#1799,#1798,#1637,.T.);
#2106=EDGE_CURVE('',#1800,#1798,#1065,.T.);
#2107=EDGE_CURVE('',#1801,#1800,#1638,.T.);
#2108=EDGE_CURVE('',#1799,#1801,#1066,.T.);
#2109=EDGE_CURVE('',#1802,#1803,#1067,.T.);
#2110=EDGE_CURVE('',#1802,#1804,#1639,.T.);
#2111=EDGE_CURVE('',#1805,#1804,#1068,.T.);
#2112=EDGE_CURVE('',#1803,#1805,#1640,.T.);
#2113=EDGE_CURVE('',#1804,#1802,#1069,.T.);
#2114=EDGE_CURVE('',#1800,#1806,#1070,.T.);
#2115=EDGE_CURVE('',#1807,#1806,#1071,.T.);
#2116=EDGE_CURVE('',#1807,#1808,#1072,.T.);
#2117=EDGE_CURVE('',#1809,#1808,#1073,.T.);
#2118=EDGE_CURVE('',#1809,#1801,#1074,.T.);
#2119=EDGE_CURVE('',#1810,#1810,#1641,.T.);
#2120=EDGE_CURVE('',#1811,#1809,#1075,.T.);
#2121=EDGE_CURVE('',#1811,#1812,#1076,.T.);
#2122=EDGE_CURVE('',#1806,#1812,#1077,.T.);
#2123=EDGE_CURVE('',#1813,#1813,#1642,.T.);
#2124=EDGE_CURVE('',#1814,#1815,#1078,.T.);
#2125=EDGE_CURVE('',#1816,#1815,#1079,.T.);
#2126=EDGE_CURVE('',#1803,#1816,#1080,.T.);
#2127=EDGE_CURVE('',#1817,#1805,#1081,.T.);
#2128=EDGE_CURVE('',#1814,#1817,#1082,.T.);
#2129=EDGE_CURVE('',#1818,#1818,#1643,.T.);
#2130=EDGE_CURVE('',#1819,#1819,#1644,.T.);
#2131=EDGE_CURVE('',#1819,#1820,#1083,.T.);
#2132=EDGE_CURVE('',#1820,#1820,#1645,.T.);
#2133=EDGE_CURVE('',#1813,#1821,#1084,.T.);
#2134=EDGE_CURVE('',#1821,#1821,#1646,.T.);
#2135=EDGE_CURVE('',#1822,#1822,#1647,.T.);
#2136=EDGE_CURVE('',#1822,#1810,#1085,.T.);
#2137=EDGE_CURVE('',#1823,#1823,#1648,.T.);
#2138=EDGE_CURVE('',#1823,#1818,#1086,.T.);
#2139=EDGE_CURVE('',#1824,#1824,#1649,.T.);
#2140=EDGE_CURVE('',#1824,#1825,#1087,.T.);
#2141=EDGE_CURVE('',#1825,#1825,#1650,.T.);
#2142=EDGE_CURVE('',#1808,#1826,#1088,.T.);
#2143=EDGE_CURVE('',#1826,#1827,#1089,.T.);
#2144=EDGE_CURVE('',#1827,#1814,#1090,.T.);
#2145=EDGE_CURVE('',#1817,#1828,#1091,.T.);
#2146=EDGE_CURVE('',#1828,#1829,#1092,.T.);
#2147=EDGE_CURVE('',#1829,#1830,#1093,.T.);
#2148=EDGE_CURVE('',#1830,#1831,#1094,.T.);
#2149=EDGE_CURVE('',#1831,#1832,#1095,.T.);
#2150=EDGE_CURVE('',#1832,#1811,#1096,.T.);
#2151=EDGE_CURVE('',#1833,#1807,#1097,.T.);
#2152=EDGE_CURVE('',#1826,#1833,#1098,.T.);
#2153=EDGE_CURVE('',#1834,#1833,#1099,.T.);
#2154=EDGE_CURVE('',#1827,#1834,#1100,.T.);
#2155=EDGE_CURVE('',#1815,#1834,#1101,.T.);
#2156=EDGE_CURVE('',#1835,#1816,#1102,.T.);
#2157=EDGE_CURVE('',#1828,#1835,#1103,.T.);
#2158=EDGE_CURVE('',#1836,#1835,#1104,.T.);
#2159=EDGE_CURVE('',#1829,#1836,#1105,.T.);
#2160=EDGE_CURVE('',#1837,#1836,#1106,.T.);
#2161=EDGE_CURVE('',#1830,#1837,#1107,.T.);
#2162=EDGE_CURVE('',#1838,#1837,#1108,.T.);
#2163=EDGE_CURVE('',#1831,#1838,#1109,.T.);
#2164=EDGE_CURVE('',#1839,#1838,#1110,.T.);
#2165=EDGE_CURVE('',#1832,#1839,#1111,.T.);
#2166=EDGE_CURVE('',#1812,#1839,#1112,.T.);
#2167=EDGE_CURVE('',#1840,#1841,#1113,.T.);
#2168=EDGE_CURVE('',#1841,#1842,#1114,.T.);
#2169=EDGE_CURVE('',#1842,#1843,#1115,.T.);
#2170=EDGE_CURVE('',#1840,#1843,#1116,.T.);
#2171=EDGE_CURVE('',#1841,#1844,#1117,.T.);
#2172=EDGE_CURVE('',#1844,#1845,#1118,.T.);
#2173=EDGE_CURVE('',#1845,#1842,#1119,.T.);
#2174=EDGE_CURVE('',#1844,#1846,#1120,.T.);
#2175=EDGE_CURVE('',#1846,#1847,#1121,.T.);
#2176=EDGE_CURVE('',#1847,#1845,#1122,.T.);
#2177=EDGE_CURVE('',#1846,#1848,#1123,.T.);
#2178=EDGE_CURVE('',#1848,#1849,#1124,.T.);
#2179=EDGE_CURVE('',#1849,#1847,#1125,.T.);
#2180=EDGE_CURVE('',#1848,#1850,#1126,.T.);
#2181=EDGE_CURVE('',#1850,#1851,#1127,.T.);
#2182=EDGE_CURVE('',#1851,#1849,#1128,.T.);
#2183=EDGE_CURVE('',#1850,#1840,#1129,.T.);
#2184=EDGE_CURVE('',#1843,#1851,#1130,.T.);
#2185=EDGE_CURVE('',#1852,#1852,#1651,.T.);
#2186=EDGE_CURVE('',#1853,#1853,#1652,.T.);
#2187=EDGE_CURVE('',#1854,#1854,#1653,.T.);
#2188=EDGE_CURVE('',#1854,#1853,#1131,.T.);
#2189=EDGE_CURVE('',#1855,#1855,#1654,.T.);
#2190=EDGE_CURVE('',#1855,#1854,#1132,.T.);
#2191=EDGE_CURVE('',#1856,#1856,#1655,.T.);
#2192=EDGE_CURVE('',#1856,#1855,#1133,.T.);
#2193=EDGE_CURVE('',#1857,#1857,#1656,.T.);
#2194=EDGE_CURVE('',#1858,#1858,#1657,.F.);
#2195=EDGE_CURVE('',#1858,#1857,#1134,.T.);
#2196=EDGE_CURVE('',#1852,#1858,#1135,.T.);
#2197=EDGE_CURVE('',#1859,#1859,#1658,.T.);
#2198=EDGE_CURVE('',#1859,#1860,#1136,.T.);
#2199=EDGE_CURVE('',#1860,#1860,#1659,.T.);
#2200=EDGE_CURVE('',#1861,#1861,#1660,.T.);
#2201=EDGE_CURVE('',#1862,#1862,#1661,.T.);
#2202=EDGE_CURVE('',#1862,#1863,#1137,.T.);
#2203=EDGE_CURVE('',#1863,#1863,#1662,.T.);
#2204=EDGE_CURVE('',#1864,#1864,#1663,.T.);
#2205=EDGE_CURVE('',#1865,#1865,#1664,.T.);
#2206=EDGE_CURVE('',#1865,#1861,#1138,.T.);
#2207=EDGE_CURVE('',#1866,#1866,#1665,.T.);
#2208=EDGE_CURVE('',#1866,#1864,#1139,.T.);
#2209=EDGE_CURVE('',#1867,#1868,#1140,.T.);
#2210=EDGE_CURVE('',#1868,#1869,#1141,.T.);
#2211=EDGE_CURVE('',#1870,#1869,#1142,.T.);
#2212=EDGE_CURVE('',#1867,#1870,#1143,.T.);
#2213=EDGE_CURVE('',#1871,#1867,#1144,.T.);
#2214=EDGE_CURVE('',#1872,#1870,#1145,.T.);
#2215=EDGE_CURVE('',#1871,#1872,#1146,.T.);
#2216=EDGE_CURVE('',#1873,#1871,#1147,.T.);
#2217=EDGE_CURVE('',#1874,#1872,#1148,.T.);
#2218=EDGE_CURVE('',#1873,#1874,#1149,.T.);
#2219=EDGE_CURVE('',#1868,#1873,#1150,.T.);
#2220=EDGE_CURVE('',#1869,#1874,#1151,.T.);
#2221=EDGE_CURVE('',#1875,#1876,#1152,.T.);
#2222=EDGE_CURVE('',#1876,#1877,#1153,.T.);
#2223=EDGE_CURVE('',#1878,#1877,#1154,.T.);
#2224=EDGE_CURVE('',#1875,#1878,#1155,.T.);
#2225=EDGE_CURVE('',#1879,#1875,#1156,.T.);
#2226=EDGE_CURVE('',#1880,#1878,#1157,.T.);
#2227=EDGE_CURVE('',#1879,#1880,#1158,.T.);
#2228=EDGE_CURVE('',#1881,#1879,#1159,.T.);
#2229=EDGE_CURVE('',#1882,#1880,#1160,.T.);
#2230=EDGE_CURVE('',#1881,#1882,#1161,.T.);
#2231=EDGE_CURVE('',#1876,#1881,#1162,.T.);
#2232=EDGE_CURVE('',#1877,#1882,#1163,.T.);
#2233=EDGE_CURVE('',#1883,#1883,#1666,.T.);
#2234=EDGE_CURVE('',#1883,#1884,#1164,.T.);
#2235=EDGE_CURVE('',#1884,#1884,#1667,.T.);
#2236=EDGE_CURVE('',#1885,#1885,#1668,.T.);
#2237=EDGE_CURVE('',#1885,#1886,#1165,.T.);
#2238=EDGE_CURVE('',#1886,#1886,#1669,.T.);
#2239=EDGE_CURVE('',#1887,#1887,#1670,.T.);
#2240=EDGE_CURVE('',#1887,#1888,#1166,.T.);
#2241=EDGE_CURVE('',#1888,#1888,#1671,.T.);
#2242=EDGE_CURVE('',#1889,#1889,#1672,.T.);
#2243=EDGE_CURVE('',#1889,#1890,#1167,.T.);
#2244=EDGE_CURVE('',#1890,#1890,#1673,.T.);
#2245=EDGE_CURVE('',#1891,#1891,#1674,.T.);
#2246=EDGE_CURVE('',#1891,#1892,#1168,.T.);
#2247=EDGE_CURVE('',#1892,#1892,#1675,.T.);
#2248=EDGE_CURVE('',#1893,#1893,#1676,.T.);
#2249=EDGE_CURVE('',#1893,#1894,#1169,.T.);
#2250=EDGE_CURVE('',#1894,#1894,#1677,.T.);
#2251=EDGE_CURVE('',#1895,#1895,#1678,.T.);
#2252=EDGE_CURVE('',#1895,#1896,#1170,.T.);
#2253=EDGE_CURVE('',#1896,#1896,#1679,.T.);
#2254=EDGE_CURVE('',#1897,#1897,#1680,.T.);
#2255=EDGE_CURVE('',#1897,#1898,#1171,.T.);
#2256=EDGE_CURVE('',#1898,#1898,#1681,.T.);
#2257=EDGE_CURVE('',#1899,#1899,#1682,.T.);
#2258=EDGE_CURVE('',#1899,#1900,#1172,.T.);
#2259=EDGE_CURVE('',#1900,#1900,#1683,.T.);
#2260=EDGE_CURVE('',#1901,#1901,#1684,.T.);
#2261=EDGE_CURVE('',#1901,#1902,#1173,.T.);
#2262=EDGE_CURVE('',#1902,#1902,#1685,.T.);
#2263=EDGE_CURVE('',#1903,#1904,#1174,.T.);
#2264=EDGE_CURVE('',#1904,#1905,#1175,.T.);
#2265=EDGE_CURVE('',#1906,#1905,#1176,.T.);
#2266=EDGE_CURVE('',#1903,#1906,#1177,.T.);
#2267=EDGE_CURVE('',#1907,#1903,#1178,.T.);
#2268=EDGE_CURVE('',#1908,#1906,#1179,.T.);
#2269=EDGE_CURVE('',#1907,#1908,#1180,.T.);
#2270=EDGE_CURVE('',#1909,#1907,#1181,.T.);
#2271=EDGE_CURVE('',#1910,#1908,#1182,.T.);
#2272=EDGE_CURVE('',#1909,#1910,#1183,.T.);
#2273=EDGE_CURVE('',#1904,#1909,#1184,.T.);
#2274=EDGE_CURVE('',#1905,#1910,#1185,.T.);
#2275=EDGE_CURVE('',#1911,#1911,#1686,.T.);
#2276=EDGE_CURVE('',#1911,#1912,#1186,.T.);
#2277=EDGE_CURVE('',#1912,#1912,#1687,.T.);
#2278=EDGE_CURVE('',#1913,#1913,#1688,.T.);
#2279=EDGE_CURVE('',#1913,#1914,#1187,.T.);
#2280=EDGE_CURVE('',#1914,#1914,#1689,.T.);
#2281=EDGE_CURVE('',#1915,#1915,#1690,.T.);
#2282=EDGE_CURVE('',#1915,#1916,#1188,.T.);
#2283=EDGE_CURVE('',#1916,#1916,#1691,.T.);
#2284=EDGE_CURVE('',#1917,#1917,#1692,.T.);
#2285=EDGE_CURVE('',#1917,#1918,#1189,.T.);
#2286=EDGE_CURVE('',#1918,#1918,#1693,.T.);
#2287=EDGE_CURVE('',#1919,#1919,#1694,.T.);
#2288=EDGE_CURVE('',#1919,#1920,#1190,.T.);
#2289=EDGE_CURVE('',#1920,#1920,#1695,.T.);
#2290=EDGE_CURVE('',#1921,#1922,#1191,.T.);
#2291=EDGE_CURVE('',#1922,#1923,#1192,.T.);
#2292=EDGE_CURVE('',#1924,#1923,#1193,.T.);
#2293=EDGE_CURVE('',#1921,#1924,#1194,.T.);
#2294=EDGE_CURVE('',#1925,#1921,#1195,.T.);
#2295=EDGE_CURVE('',#1926,#1924,#1196,.T.);
#2296=EDGE_CURVE('',#1925,#1926,#1197,.T.);
#2297=EDGE_CURVE('',#1927,#1925,#1198,.T.);
#2298=EDGE_CURVE('',#1928,#1926,#1199,.T.);
#2299=EDGE_CURVE('',#1927,#1928,#1200,.T.);
#2300=EDGE_CURVE('',#1922,#1927,#1201,.T.);
#2301=EDGE_CURVE('',#1923,#1928,#1202,.T.);
#2302=EDGE_CURVE('',#1929,#1930,#1696,.T.);
#2303=EDGE_CURVE('',#1931,#1929,#1203,.T.);
#2304=EDGE_CURVE('',#1932,#1931,#1204,.T.);
#2305=EDGE_CURVE('',#1930,#1932,#1205,.T.);
#2306=EDGE_CURVE('',#1930,#1933,#1206,.T.);
#2307=EDGE_CURVE('',#1934,#1932,#1207,.T.);
#2308=EDGE_CURVE('',#1934,#1933,#1208,.T.);
#2309=EDGE_CURVE('',#1933,#1935,#1697,.T.);
#2310=EDGE_CURVE('',#1936,#1934,#1209,.T.);
#2311=EDGE_CURVE('',#1935,#1936,#1210,.T.);
#2312=EDGE_CURVE('',#1935,#1929,#1211,.T.);
#2313=EDGE_CURVE('',#1936,#1931,#1212,.T.);
#2314=EDGE_CURVE('',#1937,#1937,#1698,.T.);
#2315=EDGE_CURVE('',#1938,#1938,#1699,.T.);
#2316=EDGE_CURVE('',#1939,#1939,#1700,.T.);
#2317=EDGE_CURVE('',#1939,#1937,#1213,.T.);
#2318=EDGE_CURVE('',#1940,#1940,#1701,.T.);
#2319=EDGE_CURVE('',#1941,#1941,#1702,.T.);
#2320=EDGE_CURVE('',#1941,#1940,#1214,.T.);
#2321=EDGE_CURVE('',#1942,#1942,#1703,.T.);
#2322=EDGE_CURVE('',#1943,#1943,#1704,.T.);
#2323=EDGE_CURVE('',#1943,#1942,#1215,.T.);
#2324=EDGE_CURVE('',#1944,#1944,#1705,.T.);
#2325=EDGE_CURVE('',#1945,#1945,#1706,.T.);
#2326=EDGE_CURVE('',#1945,#1944,#1216,.T.);
#2327=EDGE_CURVE('',#1946,#1946,#1707,.T.);
#2328=EDGE_CURVE('',#1947,#1947,#1708,.T.);
#2329=EDGE_CURVE('',#1947,#1946,#1217,.T.);
#2330=EDGE_CURVE('',#1948,#1948,#1709,.T.);
#2331=EDGE_CURVE('',#1948,#1938,#1218,.T.);
#2332=EDGE_CURVE('',#1949,#1950,#1710,.T.);
#2333=EDGE_CURVE('',#1951,#1949,#1219,.T.);
#2334=EDGE_CURVE('',#1952,#1951,#1711,.T.);
#2335=EDGE_CURVE('',#1950,#1952,#1220,.T.);
#2336=EDGE_CURVE('',#1950,#1953,#1221,.T.);
#2337=EDGE_CURVE('',#1954,#1952,#1222,.T.);
#2338=EDGE_CURVE('',#1954,#1953,#1223,.T.);
#2339=EDGE_CURVE('',#1953,#1955,#1712,.T.);
#2340=EDGE_CURVE('',#1956,#1954,#1713,.T.);
#2341=EDGE_CURVE('',#1955,#1956,#1224,.T.);
#2342=EDGE_CURVE('',#1955,#1949,#1225,.T.);
#2343=EDGE_CURVE('',#1951,#1956,#1226,.T.);
#2344=EDGE_CURVE('',#1957,#1957,#1714,.T.);
#2345=EDGE_CURVE('',#1958,#1958,#1715,.T.);
#2346=EDGE_CURVE('',#1959,#1959,#1716,.T.);
#2347=EDGE_CURVE('',#1959,#1957,#1227,.T.);
#2348=EDGE_CURVE('',#1960,#1960,#1717,.T.);
#2349=EDGE_CURVE('',#1960,#1958,#1228,.T.);
#2350=EDGE_CURVE('',#1961,#1961,#1718,.T.);
#2351=EDGE_CURVE('',#1961,#1962,#1229,.T.);
#2352=EDGE_CURVE('',#1962,#1962,#1719,.T.);
#2353=EDGE_CURVE('',#1963,#1963,#1720,.T.);
#2354=EDGE_CURVE('',#1963,#1964,#1230,.T.);
#2355=EDGE_CURVE('',#1964,#1964,#1721,.T.);
#2356=EDGE_CURVE('',#1965,#1965,#1722,.T.);
#2357=EDGE_CURVE('',#1965,#1966,#1231,.T.);
#2358=EDGE_CURVE('',#1966,#1966,#1723,.T.);
#2359=EDGE_CURVE('',#1967,#1967,#1724,.T.);
#2360=EDGE_CURVE('',#1967,#1968,#1232,.T.);
#2361=EDGE_CURVE('',#1968,#1968,#1725,.T.);
#2362=EDGE_CURVE('',#1969,#1969,#1726,.T.);
#2363=EDGE_CURVE('',#1969,#1970,#1233,.T.);
#2364=EDGE_CURVE('',#1970,#1970,#1727,.T.);
#2365=EDGE_CURVE('',#1971,#1971,#1728,.T.);
#2366=EDGE_CURVE('',#1971,#1972,#1234,.T.);
#2367=EDGE_CURVE('',#1972,#1972,#1729,.T.);
#2368=EDGE_CURVE('',#1973,#1974,#1235,.T.);
#2369=EDGE_CURVE('',#1974,#1975,#1236,.T.);
#2370=EDGE_CURVE('',#1976,#1975,#1237,.T.);
#2371=EDGE_CURVE('',#1973,#1976,#1238,.T.);
#2372=EDGE_CURVE('',#1977,#1973,#1239,.T.);
#2373=EDGE_CURVE('',#1978,#1976,#1240,.T.);
#2374=EDGE_CURVE('',#1977,#1978,#1241,.T.);
#2375=EDGE_CURVE('',#1979,#1977,#1242,.T.);
#2376=EDGE_CURVE('',#1980,#1978,#1243,.T.);
#2377=EDGE_CURVE('',#1979,#1980,#1244,.T.);
#2378=EDGE_CURVE('',#1974,#1979,#1245,.T.);
#2379=EDGE_CURVE('',#1975,#1980,#1246,.T.);
#2380=EDGE_CURVE('',#1981,#1981,#1730,.T.);
#2381=EDGE_CURVE('',#1982,#1982,#1731,.T.);
#2382=EDGE_CURVE('',#1982,#1981,#1247,.T.);
#2383=EDGE_CURVE('',#1983,#1983,#1732,.T.);
#2384=EDGE_CURVE('',#1983,#1982,#1248,.T.);
#2385=EDGE_CURVE('',#1984,#1984,#1733,.T.);
#2386=EDGE_CURVE('',#1984,#1983,#1249,.T.);
#2387=EDGE_CURVE('',#1985,#1985,#1734,.T.);
#2388=EDGE_CURVE('',#1986,#1986,#1735,.F.);
#2389=EDGE_CURVE('',#1986,#1985,#1250,.T.);
#2390=EDGE_CURVE('',#1987,#1987,#1736,.F.);
#2391=EDGE_CURVE('',#1987,#1986,#1251,.T.);
#2392=EDGE_CURVE('',#1988,#1988,#1737,.T.);
#2393=EDGE_CURVE('',#1988,#1987,#1252,.T.);
#2394=EDGE_CURVE('',#1989,#1990,#1253,.T.);
#2395=EDGE_CURVE('',#1990,#1991,#1254,.T.);
#2396=EDGE_CURVE('',#1991,#1992,#1255,.T.);
#2397=EDGE_CURVE('',#1989,#1992,#1256,.T.);
#2398=EDGE_CURVE('',#1990,#1993,#1257,.T.);
#2399=EDGE_CURVE('',#1993,#1994,#1258,.T.);
#2400=EDGE_CURVE('',#1994,#1991,#1259,.T.);
#2401=EDGE_CURVE('',#1993,#1995,#1260,.T.);
#2402=EDGE_CURVE('',#1995,#1996,#1261,.T.);
#2403=EDGE_CURVE('',#1996,#1994,#1262,.T.);
#2404=EDGE_CURVE('',#1995,#1997,#1263,.T.);
#2405=EDGE_CURVE('',#1997,#1998,#1264,.T.);
#2406=EDGE_CURVE('',#1998,#1996,#1265,.T.);
#2407=EDGE_CURVE('',#1997,#1999,#1266,.T.);
#2408=EDGE_CURVE('',#1999,#2000,#1267,.T.);
#2409=EDGE_CURVE('',#2000,#1998,#1268,.T.);
#2410=EDGE_CURVE('',#1999,#1989,#1269,.T.);
#2411=EDGE_CURVE('',#1992,#2000,#1270,.T.);
#2412=EDGE_CURVE('',#2001,#2001,#1738,.T.);
#2413=EDGE_CURVE('',#2002,#2002,#1739,.T.);
#2414=EDGE_CURVE('',#2002,#2001,#1271,.T.);
#2415=EDGE_CURVE('',#2003,#2003,#1740,.T.);
#2416=EDGE_CURVE('',#2003,#2002,#1272,.T.);
#2417=EDGE_CURVE('',#2004,#2004,#1741,.T.);
#2418=EDGE_CURVE('',#2004,#2003,#1273,.T.);
#2419=EDGE_CURVE('',#2005,#2005,#1742,.T.);
#2420=EDGE_CURVE('',#2006,#2006,#1743,.F.);
#2421=EDGE_CURVE('',#2006,#2005,#1274,.T.);
#2422=EDGE_CURVE('',#2007,#2007,#1744,.F.);
#2423=EDGE_CURVE('',#2007,#2006,#1275,.T.);
#2424=EDGE_CURVE('',#2008,#2008,#1745,.T.);
#2425=EDGE_CURVE('',#2008,#2007,#1276,.T.);
#2426=EDGE_CURVE('',#2009,#2010,#1277,.T.);
#2427=EDGE_CURVE('',#2010,#2011,#1278,.T.);
#2428=EDGE_CURVE('',#2011,#2012,#1279,.T.);
#2429=EDGE_CURVE('',#2009,#2012,#1280,.T.);
#2430=EDGE_CURVE('',#2010,#2013,#1281,.T.);
#2431=EDGE_CURVE('',#2013,#2014,#1282,.T.);
#2432=EDGE_CURVE('',#2014,#2011,#1283,.T.);
#2433=EDGE_CURVE('',#2013,#2015,#1284,.T.);
#2434=EDGE_CURVE('',#2015,#2016,#1285,.T.);
#2435=EDGE_CURVE('',#2016,#2014,#1286,.T.);
#2436=EDGE_CURVE('',#2015,#2017,#1287,.T.);
#2437=EDGE_CURVE('',#2017,#2018,#1288,.T.);
#2438=EDGE_CURVE('',#2018,#2016,#1289,.T.);
#2439=EDGE_CURVE('',#2017,#2019,#1290,.T.);
#2440=EDGE_CURVE('',#2019,#2020,#1291,.T.);
#2441=EDGE_CURVE('',#2020,#2018,#1292,.T.);
#2442=EDGE_CURVE('',#2019,#2009,#1293,.T.);
#2443=EDGE_CURVE('',#2012,#2020,#1294,.T.);
#2444=EDGE_CURVE('',#2021,#2021,#1746,.T.);
#2445=EDGE_CURVE('',#2021,#2022,#1295,.T.);
#2446=EDGE_CURVE('',#2022,#2022,#1747,.T.);
#2447=EDGE_CURVE('',#2023,#2023,#1748,.T.);
#2448=EDGE_CURVE('',#2023,#2024,#1296,.T.);
#2449=EDGE_CURVE('',#2024,#2024,#1749,.T.);
#2450=EDGE_CURVE('',#2025,#2025,#1750,.T.);
#2451=EDGE_CURVE('',#2025,#2026,#1297,.T.);
#2452=EDGE_CURVE('',#2026,#2026,#1751,.T.);
#2453=EDGE_CURVE('',#2027,#2027,#1752,.T.);
#2454=EDGE_CURVE('',#2027,#2028,#1298,.T.);
#2455=EDGE_CURVE('',#2028,#2028,#1753,.T.);
#2456=EDGE_CURVE('',#2029,#2029,#1754,.T.);
#2457=EDGE_CURVE('',#2030,#2030,#1755,.T.);
#2458=EDGE_CURVE('',#2030,#2029,#1299,.T.);
#2459=EDGE_CURVE('',#2031,#2031,#1756,.T.);
#2460=EDGE_CURVE('',#2031,#2030,#1300,.T.);
#2461=EDGE_CURVE('',#2032,#2032,#1757,.T.);
#2462=EDGE_CURVE('',#2032,#2031,#1301,.T.);
#2463=EDGE_CURVE('',#2033,#2033,#1758,.T.);
#2464=EDGE_CURVE('',#2034,#2034,#1759,.F.);
#2465=EDGE_CURVE('',#2034,#2033,#1302,.T.);
#2466=EDGE_CURVE('',#2035,#2035,#1760,.F.);
#2467=EDGE_CURVE('',#2035,#2034,#1303,.T.);
#2468=EDGE_CURVE('',#2036,#2036,#1761,.T.);
#2469=EDGE_CURVE('',#2036,#2035,#1304,.T.);
#2470=EDGE_CURVE('',#2037,#2038,#1305,.T.);
#2471=EDGE_CURVE('',#2038,#2039,#1306,.T.);
#2472=EDGE_CURVE('',#2039,#2040,#1307,.T.);
#2473=EDGE_CURVE('',#2037,#2040,#1308,.T.);
#2474=EDGE_CURVE('',#2038,#2041,#1309,.T.);
#2475=EDGE_CURVE('',#2041,#2042,#1310,.T.);
#2476=EDGE_CURVE('',#2042,#2039,#1311,.T.);
#2477=EDGE_CURVE('',#2041,#2043,#1312,.T.);
#2478=EDGE_CURVE('',#2043,#2044,#1313,.T.);
#2479=EDGE_CURVE('',#2044,#2042,#1314,.T.);
#2480=EDGE_CURVE('',#2043,#2045,#1315,.T.);
#2481=EDGE_CURVE('',#2045,#2046,#1316,.T.);
#2482=EDGE_CURVE('',#2046,#2044,#1317,.T.);
#2483=EDGE_CURVE('',#2045,#2047,#1318,.T.);
#2484=EDGE_CURVE('',#2047,#2048,#1319,.T.);
#2485=EDGE_CURVE('',#2048,#2046,#1320,.T.);
#2486=EDGE_CURVE('',#2047,#2037,#1321,.T.);
#2487=EDGE_CURVE('',#2040,#2048,#1322,.T.);
#2488=ORIENTED_EDGE('',*,*,#2049,.F.);
#2489=ORIENTED_EDGE('',*,*,#2050,.T.);
#2490=ORIENTED_EDGE('',*,*,#2051,.F.);
#2491=ORIENTED_EDGE('',*,*,#2050,.F.);
#2492=ORIENTED_EDGE('',*,*,#2052,.F.);
#2493=ORIENTED_EDGE('',*,*,#2053,.T.);
#2494=ORIENTED_EDGE('',*,*,#2054,.F.);
#2495=ORIENTED_EDGE('',*,*,#2053,.F.);
#2496=ORIENTED_EDGE('',*,*,#2055,.F.);
#2497=ORIENTED_EDGE('',*,*,#2056,.T.);
#2498=ORIENTED_EDGE('',*,*,#2057,.F.);
#2499=ORIENTED_EDGE('',*,*,#2056,.F.);
#2500=ORIENTED_EDGE('',*,*,#2058,.F.);
#2501=ORIENTED_EDGE('',*,*,#2059,.T.);
#2502=ORIENTED_EDGE('',*,*,#2060,.F.);
#2503=ORIENTED_EDGE('',*,*,#2059,.F.);
#2504=ORIENTED_EDGE('',*,*,#2061,.F.);
#2505=ORIENTED_EDGE('',*,*,#2062,.T.);
#2506=ORIENTED_EDGE('',*,*,#2063,.F.);
#2507=ORIENTED_EDGE('',*,*,#2062,.F.);
#2508=ORIENTED_EDGE('',*,*,#2064,.F.);
#2509=ORIENTED_EDGE('',*,*,#2065,.T.);
#2510=ORIENTED_EDGE('',*,*,#2066,.F.);
#2511=ORIENTED_EDGE('',*,*,#2065,.F.);
#2512=ORIENTED_EDGE('',*,*,#2067,.F.);
#2513=ORIENTED_EDGE('',*,*,#2068,.T.);
#2514=ORIENTED_EDGE('',*,*,#2069,.F.);
#2515=ORIENTED_EDGE('',*,*,#2068,.F.);
#2516=ORIENTED_EDGE('',*,*,#2070,.F.);
#2517=ORIENTED_EDGE('',*,*,#2071,.T.);
#2518=ORIENTED_EDGE('',*,*,#2072,.F.);
#2519=ORIENTED_EDGE('',*,*,#2071,.F.);
#2520=ORIENTED_EDGE('',*,*,#2073,.F.);
#2521=ORIENTED_EDGE('',*,*,#2074,.T.);
#2522=ORIENTED_EDGE('',*,*,#2075,.F.);
#2523=ORIENTED_EDGE('',*,*,#2074,.F.);
#2524=ORIENTED_EDGE('',*,*,#2076,.F.);
#2525=ORIENTED_EDGE('',*,*,#2077,.T.);
#2526=ORIENTED_EDGE('',*,*,#2078,.F.);
#2527=ORIENTED_EDGE('',*,*,#2077,.F.);
#2528=ORIENTED_EDGE('',*,*,#2079,.F.);
#2529=ORIENTED_EDGE('',*,*,#2080,.T.);
#2530=ORIENTED_EDGE('',*,*,#2081,.F.);
#2531=ORIENTED_EDGE('',*,*,#2080,.F.);
#2532=ORIENTED_EDGE('',*,*,#2082,.F.);
#2533=ORIENTED_EDGE('',*,*,#2083,.T.);
#2534=ORIENTED_EDGE('',*,*,#2084,.F.);
#2535=ORIENTED_EDGE('',*,*,#2083,.F.);
#2536=ORIENTED_EDGE('',*,*,#2085,.T.);
#2537=ORIENTED_EDGE('',*,*,#2086,.T.);
#2538=ORIENTED_EDGE('',*,*,#2087,.F.);
#2539=ORIENTED_EDGE('',*,*,#2088,.F.);
#2540=ORIENTED_EDGE('',*,*,#2089,.T.);
#2541=ORIENTED_EDGE('',*,*,#2088,.T.);
#2542=ORIENTED_EDGE('',*,*,#2090,.F.);
#2543=ORIENTED_EDGE('',*,*,#2091,.F.);
#2544=ORIENTED_EDGE('',*,*,#2092,.T.);
#2545=ORIENTED_EDGE('',*,*,#2091,.T.);
#2546=ORIENTED_EDGE('',*,*,#2093,.F.);
#2547=ORIENTED_EDGE('',*,*,#2094,.F.);
#2548=ORIENTED_EDGE('',*,*,#2095,.T.);
#2549=ORIENTED_EDGE('',*,*,#2094,.T.);
#2550=ORIENTED_EDGE('',*,*,#2096,.F.);
#2551=ORIENTED_EDGE('',*,*,#2086,.F.);
#2552=ORIENTED_EDGE('',*,*,#2096,.T.);
#2553=ORIENTED_EDGE('',*,*,#2093,.T.);
#2554=ORIENTED_EDGE('',*,*,#2090,.T.);
#2555=ORIENTED_EDGE('',*,*,#2087,.T.);
#2556=ORIENTED_EDGE('',*,*,#2063,.T.);
#2557=ORIENTED_EDGE('',*,*,#2066,.T.);
#2558=ORIENTED_EDGE('',*,*,#2069,.T.);
#2559=ORIENTED_EDGE('',*,*,#2072,.T.);
#2560=ORIENTED_EDGE('',*,*,#2075,.T.);
#2561=ORIENTED_EDGE('',*,*,#2078,.T.);
#2562=ORIENTED_EDGE('',*,*,#2081,.T.);
#2563=ORIENTED_EDGE('',*,*,#2084,.T.);
#2564=ORIENTED_EDGE('',*,*,#2060,.T.);
#2565=ORIENTED_EDGE('',*,*,#2057,.T.);
#2566=ORIENTED_EDGE('',*,*,#2054,.T.);
#2567=ORIENTED_EDGE('',*,*,#2051,.T.);
#2568=ORIENTED_EDGE('',*,*,#2095,.F.);
#2569=ORIENTED_EDGE('',*,*,#2085,.F.);
#2570=ORIENTED_EDGE('',*,*,#2089,.F.);
#2571=ORIENTED_EDGE('',*,*,#2092,.F.);
#2572=ORIENTED_EDGE('',*,*,#2061,.T.);
#2573=ORIENTED_EDGE('',*,*,#2064,.T.);
#2574=ORIENTED_EDGE('',*,*,#2067,.T.);
#2575=ORIENTED_EDGE('',*,*,#2070,.T.);
#2576=ORIENTED_EDGE('',*,*,#2073,.T.);
#2577=ORIENTED_EDGE('',*,*,#2076,.T.);
#2578=ORIENTED_EDGE('',*,*,#2079,.T.);
#2579=ORIENTED_EDGE('',*,*,#2082,.T.);
#2580=ORIENTED_EDGE('',*,*,#2058,.T.);
#2581=ORIENTED_EDGE('',*,*,#2055,.T.);
#2582=ORIENTED_EDGE('',*,*,#2052,.T.);
#2583=ORIENTED_EDGE('',*,*,#2049,.T.);
#2584=ORIENTED_EDGE('',*,*,#2097,.T.);
#2585=ORIENTED_EDGE('',*,*,#2098,.T.);
#2586=ORIENTED_EDGE('',*,*,#2099,.T.);
#2587=ORIENTED_EDGE('',*,*,#2098,.F.);
#2588=ORIENTED_EDGE('',*,*,#2100,.F.);
#2589=ORIENTED_EDGE('',*,*,#2101,.T.);
#2590=ORIENTED_EDGE('',*,*,#2097,.F.);
#2591=ORIENTED_EDGE('',*,*,#2101,.F.);
#2592=ORIENTED_EDGE('',*,*,#2099,.F.);
#2593=ORIENTED_EDGE('',*,*,#2102,.T.);
#2594=ORIENTED_EDGE('',*,*,#2103,.T.);
#2595=ORIENTED_EDGE('',*,*,#2100,.T.);
#2596=ORIENTED_EDGE('',*,*,#2103,.F.);
#2597=ORIENTED_EDGE('',*,*,#2102,.F.);
#2598=ORIENTED_EDGE('',*,*,#2104,.F.);
#2599=ORIENTED_EDGE('',*,*,#2105,.F.);
#2600=ORIENTED_EDGE('',*,*,#2106,.F.);
#2601=ORIENTED_EDGE('',*,*,#2107,.F.);
#2602=ORIENTED_EDGE('',*,*,#2108,.F.);
#2603=ORIENTED_EDGE('',*,*,#2105,.T.);
#2604=ORIENTED_EDGE('',*,*,#2109,.F.);
#2605=ORIENTED_EDGE('',*,*,#2110,.T.);
#2606=ORIENTED_EDGE('',*,*,#2111,.F.);
#2607=ORIENTED_EDGE('',*,*,#2112,.F.);
#2608=ORIENTED_EDGE('',*,*,#2113,.F.);
#2609=ORIENTED_EDGE('',*,*,#2110,.F.);
#2610=ORIENTED_EDGE('',*,*,#2114,.T.);
#2611=ORIENTED_EDGE('',*,*,#2115,.F.);
#2612=ORIENTED_EDGE('',*,*,#2116,.T.);
#2613=ORIENTED_EDGE('',*,*,#2117,.F.);
#2614=ORIENTED_EDGE('',*,*,#2118,.T.);
#2615=ORIENTED_EDGE('',*,*,#2107,.T.);
#2616=ORIENTED_EDGE('',*,*,#2119,.T.);
#2617=ORIENTED_EDGE('',*,*,#2106,.T.);
#2618=ORIENTED_EDGE('',*,*,#2104,.T.);
#2619=ORIENTED_EDGE('',*,*,#2108,.T.);
#2620=ORIENTED_EDGE('',*,*,#2118,.F.);
#2621=ORIENTED_EDGE('',*,*,#2120,.F.);
#2622=ORIENTED_EDGE('',*,*,#2121,.T.);
#2623=ORIENTED_EDGE('',*,*,#2122,.F.);
#2624=ORIENTED_EDGE('',*,*,#2114,.F.);
#2625=ORIENTED_EDGE('',*,*,#2123,.T.);
#2626=ORIENTED_EDGE('',*,*,#2124,.T.);
#2627=ORIENTED_EDGE('',*,*,#2125,.F.);
#2628=ORIENTED_EDGE('',*,*,#2126,.F.);
#2629=ORIENTED_EDGE('',*,*,#2112,.T.);
#2630=ORIENTED_EDGE('',*,*,#2127,.F.);
#2631=ORIENTED_EDGE('',*,*,#2128,.F.);
#2632=ORIENTED_EDGE('',*,*,#2129,.T.);
#2633=ORIENTED_EDGE('',*,*,#2130,.F.);
#2634=ORIENTED_EDGE('',*,*,#2131,.T.);
#2635=ORIENTED_EDGE('',*,*,#2132,.F.);
#2636=ORIENTED_EDGE('',*,*,#2131,.F.);
#2637=ORIENTED_EDGE('',*,*,#2123,.F.);
#2638=ORIENTED_EDGE('',*,*,#2133,.T.);
#2639=ORIENTED_EDGE('',*,*,#2134,.F.);
#2640=ORIENTED_EDGE('',*,*,#2133,.F.);
#2641=ORIENTED_EDGE('',*,*,#2135,.F.);
#2642=ORIENTED_EDGE('',*,*,#2136,.T.);
#2643=ORIENTED_EDGE('',*,*,#2119,.F.);
#2644=ORIENTED_EDGE('',*,*,#2136,.F.);
#2645=ORIENTED_EDGE('',*,*,#2137,.F.);
#2646=ORIENTED_EDGE('',*,*,#2138,.T.);
#2647=ORIENTED_EDGE('',*,*,#2129,.F.);
#2648=ORIENTED_EDGE('',*,*,#2138,.F.);
#2649=ORIENTED_EDGE('',*,*,#2139,.F.);
#2650=ORIENTED_EDGE('',*,*,#2140,.T.);
#2651=ORIENTED_EDGE('',*,*,#2141,.F.);
#2652=ORIENTED_EDGE('',*,*,#2140,.F.);
#2653=ORIENTED_EDGE('',*,*,#2117,.T.);
#2654=ORIENTED_EDGE('',*,*,#2142,.T.);
#2655=ORIENTED_EDGE('',*,*,#2143,.T.);
#2656=ORIENTED_EDGE('',*,*,#2144,.T.);
#2657=ORIENTED_EDGE('',*,*,#2128,.T.);
#2658=ORIENTED_EDGE('',*,*,#2145,.T.);
#2659=ORIENTED_EDGE('',*,*,#2146,.T.);
#2660=ORIENTED_EDGE('',*,*,#2147,.T.);
#2661=ORIENTED_EDGE('',*,*,#2148,.T.);
#2662=ORIENTED_EDGE('',*,*,#2149,.T.);
#2663=ORIENTED_EDGE('',*,*,#2150,.T.);
#2664=ORIENTED_EDGE('',*,*,#2120,.T.);
#2665=ORIENTED_EDGE('',*,*,#2139,.T.);
#2666=ORIENTED_EDGE('',*,*,#2116,.F.);
#2667=ORIENTED_EDGE('',*,*,#2151,.F.);
#2668=ORIENTED_EDGE('',*,*,#2152,.F.);
#2669=ORIENTED_EDGE('',*,*,#2142,.F.);
#2670=ORIENTED_EDGE('',*,*,#2152,.T.);
#2671=ORIENTED_EDGE('',*,*,#2153,.F.);
#2672=ORIENTED_EDGE('',*,*,#2154,.F.);
#2673=ORIENTED_EDGE('',*,*,#2143,.F.);
#2674=ORIENTED_EDGE('',*,*,#2135,.T.);
#2675=ORIENTED_EDGE('',*,*,#2137,.T.);
#2676=ORIENTED_EDGE('',*,*,#2154,.T.);
#2677=ORIENTED_EDGE('',*,*,#2155,.F.);
#2678=ORIENTED_EDGE('',*,*,#2124,.F.);
#2679=ORIENTED_EDGE('',*,*,#2144,.F.);
#2680=ORIENTED_EDGE('',*,*,#2109,.T.);
#2681=ORIENTED_EDGE('',*,*,#2126,.T.);
#2682=ORIENTED_EDGE('',*,*,#2156,.F.);
#2683=ORIENTED_EDGE('',*,*,#2157,.F.);
#2684=ORIENTED_EDGE('',*,*,#2145,.F.);
#2685=ORIENTED_EDGE('',*,*,#2127,.T.);
#2686=ORIENTED_EDGE('',*,*,#2111,.T.);
#2687=ORIENTED_EDGE('',*,*,#2113,.T.);
#2688=ORIENTED_EDGE('',*,*,#2132,.T.);
#2689=ORIENTED_EDGE('',*,*,#2157,.T.);
#2690=ORIENTED_EDGE('',*,*,#2158,.F.);
#2691=ORIENTED_EDGE('',*,*,#2159,.F.);
#2692=ORIENTED_EDGE('',*,*,#2146,.F.);
#2693=ORIENTED_EDGE('',*,*,#2159,.T.);
#2694=ORIENTED_EDGE('',*,*,#2160,.F.);
#2695=ORIENTED_EDGE('',*,*,#2161,.F.);
#2696=ORIENTED_EDGE('',*,*,#2147,.F.);
#2697=ORIENTED_EDGE('',*,*,#2130,.T.);
#2698=ORIENTED_EDGE('',*,*,#2161,.T.);
#2699=ORIENTED_EDGE('',*,*,#2162,.F.);
#2700=ORIENTED_EDGE('',*,*,#2163,.F.);
#2701=ORIENTED_EDGE('',*,*,#2148,.F.);
#2702=ORIENTED_EDGE('',*,*,#2163,.T.);
#2703=ORIENTED_EDGE('',*,*,#2164,.F.);
#2704=ORIENTED_EDGE('',*,*,#2165,.F.);
#2705=ORIENTED_EDGE('',*,*,#2149,.F.);
#2706=ORIENTED_EDGE('',*,*,#2134,.T.);
#2707=ORIENTED_EDGE('',*,*,#2165,.T.);
#2708=ORIENTED_EDGE('',*,*,#2166,.F.);
#2709=ORIENTED_EDGE('',*,*,#2121,.F.);
#2710=ORIENTED_EDGE('',*,*,#2150,.F.);
#2711=ORIENTED_EDGE('',*,*,#2115,.T.);
#2712=ORIENTED_EDGE('',*,*,#2122,.T.);
#2713=ORIENTED_EDGE('',*,*,#2166,.T.);
#2714=ORIENTED_EDGE('',*,*,#2164,.T.);
#2715=ORIENTED_EDGE('',*,*,#2162,.T.);
#2716=ORIENTED_EDGE('',*,*,#2160,.T.);
#2717=ORIENTED_EDGE('',*,*,#2158,.T.);
#2718=ORIENTED_EDGE('',*,*,#2156,.T.);
#2719=ORIENTED_EDGE('',*,*,#2125,.T.);
#2720=ORIENTED_EDGE('',*,*,#2155,.T.);
#2721=ORIENTED_EDGE('',*,*,#2153,.T.);
#2722=ORIENTED_EDGE('',*,*,#2151,.T.);
#2723=ORIENTED_EDGE('',*,*,#2141,.T.);
#2724=ORIENTED_EDGE('',*,*,#2167,.T.);
#2725=ORIENTED_EDGE('',*,*,#2168,.T.);
#2726=ORIENTED_EDGE('',*,*,#2169,.T.);
#2727=ORIENTED_EDGE('',*,*,#2170,.F.);
#2728=ORIENTED_EDGE('',*,*,#2171,.T.);
#2729=ORIENTED_EDGE('',*,*,#2172,.T.);
#2730=ORIENTED_EDGE('',*,*,#2173,.T.);
#2731=ORIENTED_EDGE('',*,*,#2168,.F.);
#2732=ORIENTED_EDGE('',*,*,#2174,.T.);
#2733=ORIENTED_EDGE('',*,*,#2175,.T.);
#2734=ORIENTED_EDGE('',*,*,#2176,.T.);
#2735=ORIENTED_EDGE('',*,*,#2172,.F.);
#2736=ORIENTED_EDGE('',*,*,#2177,.T.);
#2737=ORIENTED_EDGE('',*,*,#2178,.T.);
#2738=ORIENTED_EDGE('',*,*,#2179,.T.);
#2739=ORIENTED_EDGE('',*,*,#2175,.F.);
#2740=ORIENTED_EDGE('',*,*,#2180,.T.);
#2741=ORIENTED_EDGE('',*,*,#2181,.T.);
#2742=ORIENTED_EDGE('',*,*,#2182,.T.);
#2743=ORIENTED_EDGE('',*,*,#2178,.F.);
#2744=ORIENTED_EDGE('',*,*,#2183,.T.);
#2745=ORIENTED_EDGE('',*,*,#2170,.T.);
#2746=ORIENTED_EDGE('',*,*,#2184,.T.);
#2747=ORIENTED_EDGE('',*,*,#2181,.F.);
#2748=ORIENTED_EDGE('',*,*,#2183,.F.);
#2749=ORIENTED_EDGE('',*,*,#2180,.F.);
#2750=ORIENTED_EDGE('',*,*,#2177,.F.);
#2751=ORIENTED_EDGE('',*,*,#2174,.F.);
#2752=ORIENTED_EDGE('',*,*,#2171,.F.);
#2753=ORIENTED_EDGE('',*,*,#2167,.F.);
#2754=ORIENTED_EDGE('',*,*,#2184,.F.);
#2755=ORIENTED_EDGE('',*,*,#2169,.F.);
#2756=ORIENTED_EDGE('',*,*,#2173,.F.);
#2757=ORIENTED_EDGE('',*,*,#2176,.F.);
#2758=ORIENTED_EDGE('',*,*,#2179,.F.);
#2759=ORIENTED_EDGE('',*,*,#2182,.F.);
#2760=ORIENTED_EDGE('',*,*,#2185,.F.);
#2761=ORIENTED_EDGE('',*,*,#2186,.F.);
#2762=ORIENTED_EDGE('',*,*,#2187,.F.);
#2763=ORIENTED_EDGE('',*,*,#2188,.T.);
#2764=ORIENTED_EDGE('',*,*,#2186,.T.);
#2765=ORIENTED_EDGE('',*,*,#2188,.F.);
#2766=ORIENTED_EDGE('',*,*,#2189,.F.);
#2767=ORIENTED_EDGE('',*,*,#2190,.T.);
#2768=ORIENTED_EDGE('',*,*,#2187,.T.);
#2769=ORIENTED_EDGE('',*,*,#2190,.F.);
#2770=ORIENTED_EDGE('',*,*,#2191,.F.);
#2771=ORIENTED_EDGE('',*,*,#2192,.T.);
#2772=ORIENTED_EDGE('',*,*,#2189,.T.);
#2773=ORIENTED_EDGE('',*,*,#2192,.F.);
#2774=ORIENTED_EDGE('',*,*,#2191,.T.);
#2775=ORIENTED_EDGE('',*,*,#2193,.F.);
#2776=ORIENTED_EDGE('',*,*,#2194,.F.);
#2777=ORIENTED_EDGE('',*,*,#2195,.T.);
#2778=ORIENTED_EDGE('',*,*,#2193,.T.);
#2779=ORIENTED_EDGE('',*,*,#2195,.F.);
#2780=ORIENTED_EDGE('',*,*,#2185,.T.);
#2781=ORIENTED_EDGE('',*,*,#2196,.T.);
#2782=ORIENTED_EDGE('',*,*,#2194,.T.);
#2783=ORIENTED_EDGE('',*,*,#2196,.F.);
#2784=ORIENTED_EDGE('',*,*,#2197,.F.);
#2785=ORIENTED_EDGE('',*,*,#2198,.T.);
#2786=ORIENTED_EDGE('',*,*,#2199,.F.);
#2787=ORIENTED_EDGE('',*,*,#2198,.F.);
#2788=ORIENTED_EDGE('',*,*,#2197,.T.);
#2789=ORIENTED_EDGE('',*,*,#2200,.F.);
#2790=ORIENTED_EDGE('',*,*,#2201,.F.);
#2791=ORIENTED_EDGE('',*,*,#2202,.T.);
#2792=ORIENTED_EDGE('',*,*,#2203,.F.);
#2793=ORIENTED_EDGE('',*,*,#2202,.F.);
#2794=ORIENTED_EDGE('',*,*,#2201,.T.);
#2795=ORIENTED_EDGE('',*,*,#2204,.F.);
#2796=ORIENTED_EDGE('',*,*,#2205,.F.);
#2797=ORIENTED_EDGE('',*,*,#2206,.T.);
#2798=ORIENTED_EDGE('',*,*,#2200,.T.);
#2799=ORIENTED_EDGE('',*,*,#2206,.F.);
#2800=ORIENTED_EDGE('',*,*,#2207,.F.);
#2801=ORIENTED_EDGE('',*,*,#2208,.T.);
#2802=ORIENTED_EDGE('',*,*,#2204,.T.);
#2803=ORIENTED_EDGE('',*,*,#2208,.F.);
#2804=ORIENTED_EDGE('',*,*,#2209,.T.);
#2805=ORIENTED_EDGE('',*,*,#2210,.T.);
#2806=ORIENTED_EDGE('',*,*,#2211,.F.);
#2807=ORIENTED_EDGE('',*,*,#2212,.F.);
#2808=ORIENTED_EDGE('',*,*,#2213,.T.);
#2809=ORIENTED_EDGE('',*,*,#2212,.T.);
#2810=ORIENTED_EDGE('',*,*,#2214,.F.);
#2811=ORIENTED_EDGE('',*,*,#2215,.F.);
#2812=ORIENTED_EDGE('',*,*,#2216,.T.);
#2813=ORIENTED_EDGE('',*,*,#2215,.T.);
#2814=ORIENTED_EDGE('',*,*,#2217,.F.);
#2815=ORIENTED_EDGE('',*,*,#2218,.F.);
#2816=ORIENTED_EDGE('',*,*,#2219,.T.);
#2817=ORIENTED_EDGE('',*,*,#2218,.T.);
#2818=ORIENTED_EDGE('',*,*,#2220,.F.);
#2819=ORIENTED_EDGE('',*,*,#2210,.F.);
#2820=ORIENTED_EDGE('',*,*,#2220,.T.);
#2821=ORIENTED_EDGE('',*,*,#2217,.T.);
#2822=ORIENTED_EDGE('',*,*,#2214,.T.);
#2823=ORIENTED_EDGE('',*,*,#2211,.T.);
#2824=ORIENTED_EDGE('',*,*,#2199,.T.);
#2825=ORIENTED_EDGE('',*,*,#2203,.T.);
#2826=ORIENTED_EDGE('',*,*,#2219,.F.);
#2827=ORIENTED_EDGE('',*,*,#2209,.F.);
#2828=ORIENTED_EDGE('',*,*,#2213,.F.);
#2829=ORIENTED_EDGE('',*,*,#2216,.F.);
#2830=ORIENTED_EDGE('',*,*,#2205,.T.);
#2831=ORIENTED_EDGE('',*,*,#2207,.T.);
#2832=ORIENTED_EDGE('',*,*,#2221,.T.);
#2833=ORIENTED_EDGE('',*,*,#2222,.T.);
#2834=ORIENTED_EDGE('',*,*,#2223,.F.);
#2835=ORIENTED_EDGE('',*,*,#2224,.F.);
#2836=ORIENTED_EDGE('',*,*,#2225,.T.);
#2837=ORIENTED_EDGE('',*,*,#2224,.T.);
#2838=ORIENTED_EDGE('',*,*,#2226,.F.);
#2839=ORIENTED_EDGE('',*,*,#2227,.F.);
#2840=ORIENTED_EDGE('',*,*,#2228,.T.);
#2841=ORIENTED_EDGE('',*,*,#2227,.T.);
#2842=ORIENTED_EDGE('',*,*,#2229,.F.);
#2843=ORIENTED_EDGE('',*,*,#2230,.F.);
#2844=ORIENTED_EDGE('',*,*,#2231,.T.);
#2845=ORIENTED_EDGE('',*,*,#2230,.T.);
#2846=ORIENTED_EDGE('',*,*,#2232,.F.);
#2847=ORIENTED_EDGE('',*,*,#2222,.F.);
#2848=ORIENTED_EDGE('',*,*,#2232,.T.);
#2849=ORIENTED_EDGE('',*,*,#2229,.T.);
#2850=ORIENTED_EDGE('',*,*,#2226,.T.);
#2851=ORIENTED_EDGE('',*,*,#2223,.T.);
#2852=ORIENTED_EDGE('',*,*,#2231,.F.);
#2853=ORIENTED_EDGE('',*,*,#2221,.F.);
#2854=ORIENTED_EDGE('',*,*,#2225,.F.);
#2855=ORIENTED_EDGE('',*,*,#2228,.F.);
#2856=ORIENTED_EDGE('',*,*,#2233,.F.);
#2857=ORIENTED_EDGE('',*,*,#2234,.T.);
#2858=ORIENTED_EDGE('',*,*,#2235,.F.);
#2859=ORIENTED_EDGE('',*,*,#2234,.F.);
#2860=ORIENTED_EDGE('',*,*,#2236,.F.);
#2861=ORIENTED_EDGE('',*,*,#2237,.T.);
#2862=ORIENTED_EDGE('',*,*,#2238,.F.);
#2863=ORIENTED_EDGE('',*,*,#2237,.F.);
#2864=ORIENTED_EDGE('',*,*,#2239,.F.);
#2865=ORIENTED_EDGE('',*,*,#2240,.T.);
#2866=ORIENTED_EDGE('',*,*,#2241,.F.);
#2867=ORIENTED_EDGE('',*,*,#2240,.F.);
#2868=ORIENTED_EDGE('',*,*,#2242,.F.);
#2869=ORIENTED_EDGE('',*,*,#2243,.T.);
#2870=ORIENTED_EDGE('',*,*,#2244,.F.);
#2871=ORIENTED_EDGE('',*,*,#2243,.F.);
#2872=ORIENTED_EDGE('',*,*,#2245,.F.);
#2873=ORIENTED_EDGE('',*,*,#2246,.T.);
#2874=ORIENTED_EDGE('',*,*,#2247,.F.);
#2875=ORIENTED_EDGE('',*,*,#2246,.F.);
#2876=ORIENTED_EDGE('',*,*,#2245,.T.);
#2877=ORIENTED_EDGE('',*,*,#2248,.F.);
#2878=ORIENTED_EDGE('',*,*,#2249,.T.);
#2879=ORIENTED_EDGE('',*,*,#2250,.F.);
#2880=ORIENTED_EDGE('',*,*,#2249,.F.);
#2881=ORIENTED_EDGE('',*,*,#2248,.T.);
#2882=ORIENTED_EDGE('',*,*,#2251,.F.);
#2883=ORIENTED_EDGE('',*,*,#2252,.T.);
#2884=ORIENTED_EDGE('',*,*,#2253,.F.);
#2885=ORIENTED_EDGE('',*,*,#2252,.F.);
#2886=ORIENTED_EDGE('',*,*,#2251,.T.);
#2887=ORIENTED_EDGE('',*,*,#2254,.F.);
#2888=ORIENTED_EDGE('',*,*,#2255,.T.);
#2889=ORIENTED_EDGE('',*,*,#2256,.F.);
#2890=ORIENTED_EDGE('',*,*,#2255,.F.);
#2891=ORIENTED_EDGE('',*,*,#2254,.T.);
#2892=ORIENTED_EDGE('',*,*,#2257,.F.);
#2893=ORIENTED_EDGE('',*,*,#2258,.T.);
#2894=ORIENTED_EDGE('',*,*,#2259,.F.);
#2895=ORIENTED_EDGE('',*,*,#2258,.F.);
#2896=ORIENTED_EDGE('',*,*,#2260,.F.);
#2897=ORIENTED_EDGE('',*,*,#2261,.T.);
#2898=ORIENTED_EDGE('',*,*,#2262,.F.);
#2899=ORIENTED_EDGE('',*,*,#2261,.F.);
#2900=ORIENTED_EDGE('',*,*,#2263,.T.);
#2901=ORIENTED_EDGE('',*,*,#2264,.T.);
#2902=ORIENTED_EDGE('',*,*,#2265,.F.);
#2903=ORIENTED_EDGE('',*,*,#2266,.F.);
#2904=ORIENTED_EDGE('',*,*,#2267,.T.);
#2905=ORIENTED_EDGE('',*,*,#2266,.T.);
#2906=ORIENTED_EDGE('',*,*,#2268,.F.);
#2907=ORIENTED_EDGE('',*,*,#2269,.F.);
#2908=ORIENTED_EDGE('',*,*,#2262,.T.);
#2909=ORIENTED_EDGE('',*,*,#2259,.T.);
#2910=ORIENTED_EDGE('',*,*,#2244,.T.);
#2911=ORIENTED_EDGE('',*,*,#2241,.T.);
#2912=ORIENTED_EDGE('',*,*,#2238,.T.);
#2913=ORIENTED_EDGE('',*,*,#2235,.T.);
#2914=ORIENTED_EDGE('',*,*,#2270,.T.);
#2915=ORIENTED_EDGE('',*,*,#2269,.T.);
#2916=ORIENTED_EDGE('',*,*,#2271,.F.);
#2917=ORIENTED_EDGE('',*,*,#2272,.F.);
#2918=ORIENTED_EDGE('',*,*,#2273,.T.);
#2919=ORIENTED_EDGE('',*,*,#2272,.T.);
#2920=ORIENTED_EDGE('',*,*,#2274,.F.);
#2921=ORIENTED_EDGE('',*,*,#2264,.F.);
#2922=ORIENTED_EDGE('',*,*,#2260,.T.);
#2923=ORIENTED_EDGE('',*,*,#2257,.T.);
#2924=ORIENTED_EDGE('',*,*,#2242,.T.);
#2925=ORIENTED_EDGE('',*,*,#2239,.T.);
#2926=ORIENTED_EDGE('',*,*,#2236,.T.);
#2927=ORIENTED_EDGE('',*,*,#2233,.T.);
#2928=ORIENTED_EDGE('',*,*,#2274,.T.);
#2929=ORIENTED_EDGE('',*,*,#2271,.T.);
#2930=ORIENTED_EDGE('',*,*,#2268,.T.);
#2931=ORIENTED_EDGE('',*,*,#2265,.T.);
#2932=ORIENTED_EDGE('',*,*,#2247,.T.);
#2933=ORIENTED_EDGE('',*,*,#2250,.T.);
#2934=ORIENTED_EDGE('',*,*,#2253,.T.);
#2935=ORIENTED_EDGE('',*,*,#2256,.T.);
#2936=ORIENTED_EDGE('',*,*,#2273,.F.);
#2937=ORIENTED_EDGE('',*,*,#2263,.F.);
#2938=ORIENTED_EDGE('',*,*,#2267,.F.);
#2939=ORIENTED_EDGE('',*,*,#2270,.F.);
#2940=ORIENTED_EDGE('',*,*,#2275,.F.);
#2941=ORIENTED_EDGE('',*,*,#2276,.T.);
#2942=ORIENTED_EDGE('',*,*,#2277,.F.);
#2943=ORIENTED_EDGE('',*,*,#2276,.F.);
#2944=ORIENTED_EDGE('',*,*,#2278,.F.);
#2945=ORIENTED_EDGE('',*,*,#2279,.T.);
#2946=ORIENTED_EDGE('',*,*,#2280,.F.);
#2947=ORIENTED_EDGE('',*,*,#2279,.F.);
#2948=ORIENTED_EDGE('',*,*,#2281,.F.);
#2949=ORIENTED_EDGE('',*,*,#2282,.T.);
#2950=ORIENTED_EDGE('',*,*,#2283,.F.);
#2951=ORIENTED_EDGE('',*,*,#2282,.F.);
#2952=ORIENTED_EDGE('',*,*,#2284,.F.);
#2953=ORIENTED_EDGE('',*,*,#2285,.T.);
#2954=ORIENTED_EDGE('',*,*,#2286,.F.);
#2955=ORIENTED_EDGE('',*,*,#2285,.F.);
#2956=ORIENTED_EDGE('',*,*,#2287,.F.);
#2957=ORIENTED_EDGE('',*,*,#2288,.T.);
#2958=ORIENTED_EDGE('',*,*,#2289,.F.);
#2959=ORIENTED_EDGE('',*,*,#2288,.F.);
#2960=ORIENTED_EDGE('',*,*,#2290,.T.);
#2961=ORIENTED_EDGE('',*,*,#2291,.T.);
#2962=ORIENTED_EDGE('',*,*,#2292,.F.);
#2963=ORIENTED_EDGE('',*,*,#2293,.F.);
#2964=ORIENTED_EDGE('',*,*,#2294,.T.);
#2965=ORIENTED_EDGE('',*,*,#2293,.T.);
#2966=ORIENTED_EDGE('',*,*,#2295,.F.);
#2967=ORIENTED_EDGE('',*,*,#2296,.F.);
#2968=ORIENTED_EDGE('',*,*,#2297,.T.);
#2969=ORIENTED_EDGE('',*,*,#2296,.T.);
#2970=ORIENTED_EDGE('',*,*,#2298,.F.);
#2971=ORIENTED_EDGE('',*,*,#2299,.F.);
#2972=ORIENTED_EDGE('',*,*,#2300,.T.);
#2973=ORIENTED_EDGE('',*,*,#2299,.T.);
#2974=ORIENTED_EDGE('',*,*,#2301,.F.);
#2975=ORIENTED_EDGE('',*,*,#2291,.F.);
#2976=ORIENTED_EDGE('',*,*,#2301,.T.);
#2977=ORIENTED_EDGE('',*,*,#2298,.T.);
#2978=ORIENTED_EDGE('',*,*,#2295,.T.);
#2979=ORIENTED_EDGE('',*,*,#2292,.T.);
#2980=ORIENTED_EDGE('',*,*,#2277,.T.);
#2981=ORIENTED_EDGE('',*,*,#2280,.T.);
#2982=ORIENTED_EDGE('',*,*,#2283,.T.);
#2983=ORIENTED_EDGE('',*,*,#2286,.T.);
#2984=ORIENTED_EDGE('',*,*,#2289,.T.);
#2985=ORIENTED_EDGE('',*,*,#2300,.F.);
#2986=ORIENTED_EDGE('',*,*,#2290,.F.);
#2987=ORIENTED_EDGE('',*,*,#2294,.F.);
#2988=ORIENTED_EDGE('',*,*,#2297,.F.);
#2989=ORIENTED_EDGE('',*,*,#2275,.T.);
#2990=ORIENTED_EDGE('',*,*,#2278,.T.);
#2991=ORIENTED_EDGE('',*,*,#2281,.T.);
#2992=ORIENTED_EDGE('',*,*,#2284,.T.);
#2993=ORIENTED_EDGE('',*,*,#2287,.T.);
#2994=ORIENTED_EDGE('',*,*,#2302,.F.);
#2995=ORIENTED_EDGE('',*,*,#2303,.F.);
#2996=ORIENTED_EDGE('',*,*,#2304,.F.);
#2997=ORIENTED_EDGE('',*,*,#2305,.F.);
#2998=ORIENTED_EDGE('',*,*,#2306,.F.);
#2999=ORIENTED_EDGE('',*,*,#2305,.T.);
#3000=ORIENTED_EDGE('',*,*,#2307,.F.);
#3001=ORIENTED_EDGE('',*,*,#2308,.T.);
#3002=ORIENTED_EDGE('',*,*,#2309,.F.);
#3003=ORIENTED_EDGE('',*,*,#2308,.F.);
#3004=ORIENTED_EDGE('',*,*,#2310,.F.);
#3005=ORIENTED_EDGE('',*,*,#2311,.F.);
#3006=ORIENTED_EDGE('',*,*,#2312,.F.);
#3007=ORIENTED_EDGE('',*,*,#2311,.T.);
#3008=ORIENTED_EDGE('',*,*,#2313,.T.);
#3009=ORIENTED_EDGE('',*,*,#2303,.T.);
#3010=ORIENTED_EDGE('',*,*,#2313,.F.);
#3011=ORIENTED_EDGE('',*,*,#2310,.T.);
#3012=ORIENTED_EDGE('',*,*,#2307,.T.);
#3013=ORIENTED_EDGE('',*,*,#2304,.T.);
#3014=ORIENTED_EDGE('',*,*,#2314,.F.);
#3015=ORIENTED_EDGE('',*,*,#2315,.T.);
#3016=ORIENTED_EDGE('',*,*,#2316,.F.);
#3017=ORIENTED_EDGE('',*,*,#2317,.T.);
#3018=ORIENTED_EDGE('',*,*,#2314,.T.);
#3019=ORIENTED_EDGE('',*,*,#2317,.F.);
#3020=ORIENTED_EDGE('',*,*,#2316,.T.);
#3021=ORIENTED_EDGE('',*,*,#2318,.F.);
#3022=ORIENTED_EDGE('',*,*,#2319,.F.);
#3023=ORIENTED_EDGE('',*,*,#2320,.T.);
#3024=ORIENTED_EDGE('',*,*,#2318,.T.);
#3025=ORIENTED_EDGE('',*,*,#2320,.F.);
#3026=ORIENTED_EDGE('',*,*,#2321,.F.);
#3027=ORIENTED_EDGE('',*,*,#2319,.T.);
#3028=ORIENTED_EDGE('',*,*,#2322,.F.);
#3029=ORIENTED_EDGE('',*,*,#2323,.T.);
#3030=ORIENTED_EDGE('',*,*,#2321,.T.);
#3031=ORIENTED_EDGE('',*,*,#2323,.F.);
#3032=ORIENTED_EDGE('',*,*,#2322,.T.);
#3033=ORIENTED_EDGE('',*,*,#2324,.F.);
#3034=ORIENTED_EDGE('',*,*,#2325,.F.);
#3035=ORIENTED_EDGE('',*,*,#2326,.T.);
#3036=ORIENTED_EDGE('',*,*,#2324,.T.);
#3037=ORIENTED_EDGE('',*,*,#2326,.F.);
#3038=ORIENTED_EDGE('',*,*,#2327,.F.);
#3039=ORIENTED_EDGE('',*,*,#2325,.T.);
#3040=ORIENTED_EDGE('',*,*,#2328,.F.);
#3041=ORIENTED_EDGE('',*,*,#2329,.T.);
#3042=ORIENTED_EDGE('',*,*,#2327,.T.);
#3043=ORIENTED_EDGE('',*,*,#2329,.F.);
#3044=ORIENTED_EDGE('',*,*,#2328,.T.);
#3045=ORIENTED_EDGE('',*,*,#2330,.F.);
#3046=ORIENTED_EDGE('',*,*,#2330,.T.);
#3047=ORIENTED_EDGE('',*,*,#2331,.T.);
#3048=ORIENTED_EDGE('',*,*,#2315,.F.);
#3049=ORIENTED_EDGE('',*,*,#2331,.F.);
#3050=ORIENTED_EDGE('',*,*,#2309,.T.);
#3051=ORIENTED_EDGE('',*,*,#2312,.T.);
#3052=ORIENTED_EDGE('',*,*,#2302,.T.);
#3053=ORIENTED_EDGE('',*,*,#2306,.T.);
#3054=ORIENTED_EDGE('',*,*,#2332,.F.);
#3055=ORIENTED_EDGE('',*,*,#2333,.F.);
#3056=ORIENTED_EDGE('',*,*,#2334,.F.);
#3057=ORIENTED_EDGE('',*,*,#2335,.F.);
#3058=ORIENTED_EDGE('',*,*,#2336,.F.);
#3059=ORIENTED_EDGE('',*,*,#2335,.T.);
#3060=ORIENTED_EDGE('',*,*,#2337,.F.);
#3061=ORIENTED_EDGE('',*,*,#2338,.T.);
#3062=ORIENTED_EDGE('',*,*,#2339,.F.);
#3063=ORIENTED_EDGE('',*,*,#2338,.F.);
#3064=ORIENTED_EDGE('',*,*,#2340,.F.);
#3065=ORIENTED_EDGE('',*,*,#2341,.F.);
#3066=ORIENTED_EDGE('',*,*,#2342,.F.);
#3067=ORIENTED_EDGE('',*,*,#2341,.T.);
#3068=ORIENTED_EDGE('',*,*,#2343,.F.);
#3069=ORIENTED_EDGE('',*,*,#2333,.T.);
#3070=ORIENTED_EDGE('',*,*,#2344,.F.);
#3071=ORIENTED_EDGE('',*,*,#2345,.T.);
#3072=ORIENTED_EDGE('',*,*,#2346,.F.);
#3073=ORIENTED_EDGE('',*,*,#2347,.T.);
#3074=ORIENTED_EDGE('',*,*,#2344,.T.);
#3075=ORIENTED_EDGE('',*,*,#2347,.F.);
#3076=ORIENTED_EDGE('',*,*,#2339,.T.);
#3077=ORIENTED_EDGE('',*,*,#2342,.T.);
#3078=ORIENTED_EDGE('',*,*,#2332,.T.);
#3079=ORIENTED_EDGE('',*,*,#2336,.T.);
#3080=ORIENTED_EDGE('',*,*,#2346,.T.);
#3081=ORIENTED_EDGE('',*,*,#2348,.F.);
#3082=ORIENTED_EDGE('',*,*,#2348,.T.);
#3083=ORIENTED_EDGE('',*,*,#2349,.T.);
#3084=ORIENTED_EDGE('',*,*,#2345,.F.);
#3085=ORIENTED_EDGE('',*,*,#2349,.F.);
#3086=ORIENTED_EDGE('',*,*,#2340,.T.);
#3087=ORIENTED_EDGE('',*,*,#2337,.T.);
#3088=ORIENTED_EDGE('',*,*,#2334,.T.);
#3089=ORIENTED_EDGE('',*,*,#2343,.T.);
#3090=ORIENTED_EDGE('',*,*,#2350,.F.);
#3091=ORIENTED_EDGE('',*,*,#2351,.T.);
#3092=ORIENTED_EDGE('',*,*,#2352,.F.);
#3093=ORIENTED_EDGE('',*,*,#2351,.F.);
#3094=ORIENTED_EDGE('',*,*,#2353,.F.);
#3095=ORIENTED_EDGE('',*,*,#2354,.T.);
#3096=ORIENTED_EDGE('',*,*,#2355,.F.);
#3097=ORIENTED_EDGE('',*,*,#2354,.F.);
#3098=ORIENTED_EDGE('',*,*,#2356,.F.);
#3099=ORIENTED_EDGE('',*,*,#2357,.T.);
#3100=ORIENTED_EDGE('',*,*,#2358,.F.);
#3101=ORIENTED_EDGE('',*,*,#2357,.F.);
#3102=ORIENTED_EDGE('',*,*,#2359,.F.);
#3103=ORIENTED_EDGE('',*,*,#2360,.T.);
#3104=ORIENTED_EDGE('',*,*,#2361,.F.);
#3105=ORIENTED_EDGE('',*,*,#2360,.F.);
#3106=ORIENTED_EDGE('',*,*,#2362,.F.);
#3107=ORIENTED_EDGE('',*,*,#2363,.T.);
#3108=ORIENTED_EDGE('',*,*,#2364,.F.);
#3109=ORIENTED_EDGE('',*,*,#2363,.F.);
#3110=ORIENTED_EDGE('',*,*,#2365,.F.);
#3111=ORIENTED_EDGE('',*,*,#2366,.T.);
#3112=ORIENTED_EDGE('',*,*,#2367,.F.);
#3113=ORIENTED_EDGE('',*,*,#2366,.F.);
#3114=ORIENTED_EDGE('',*,*,#2368,.T.);
#3115=ORIENTED_EDGE('',*,*,#2369,.T.);
#3116=ORIENTED_EDGE('',*,*,#2370,.F.);
#3117=ORIENTED_EDGE('',*,*,#2371,.F.);
#3118=ORIENTED_EDGE('',*,*,#2372,.T.);
#3119=ORIENTED_EDGE('',*,*,#2371,.T.);
#3120=ORIENTED_EDGE('',*,*,#2373,.F.);
#3121=ORIENTED_EDGE('',*,*,#2374,.F.);
#3122=ORIENTED_EDGE('',*,*,#2367,.T.);
#3123=ORIENTED_EDGE('',*,*,#2364,.T.);
#3124=ORIENTED_EDGE('',*,*,#2361,.T.);
#3125=ORIENTED_EDGE('',*,*,#2358,.T.);
#3126=ORIENTED_EDGE('',*,*,#2355,.T.);
#3127=ORIENTED_EDGE('',*,*,#2352,.T.);
#3128=ORIENTED_EDGE('',*,*,#2375,.T.);
#3129=ORIENTED_EDGE('',*,*,#2374,.T.);
#3130=ORIENTED_EDGE('',*,*,#2376,.F.);
#3131=ORIENTED_EDGE('',*,*,#2377,.F.);
#3132=ORIENTED_EDGE('',*,*,#2378,.T.);
#3133=ORIENTED_EDGE('',*,*,#2377,.T.);
#3134=ORIENTED_EDGE('',*,*,#2379,.F.);
#3135=ORIENTED_EDGE('',*,*,#2369,.F.);
#3136=ORIENTED_EDGE('',*,*,#2365,.T.);
#3137=ORIENTED_EDGE('',*,*,#2362,.T.);
#3138=ORIENTED_EDGE('',*,*,#2359,.T.);
#3139=ORIENTED_EDGE('',*,*,#2356,.T.);
#3140=ORIENTED_EDGE('',*,*,#2353,.T.);
#3141=ORIENTED_EDGE('',*,*,#2350,.T.);
#3142=ORIENTED_EDGE('',*,*,#2379,.T.);
#3143=ORIENTED_EDGE('',*,*,#2376,.T.);
#3144=ORIENTED_EDGE('',*,*,#2373,.T.);
#3145=ORIENTED_EDGE('',*,*,#2370,.T.);
#3146=ORIENTED_EDGE('',*,*,#2378,.F.);
#3147=ORIENTED_EDGE('',*,*,#2368,.F.);
#3148=ORIENTED_EDGE('',*,*,#2372,.F.);
#3149=ORIENTED_EDGE('',*,*,#2375,.F.);
#3150=ORIENTED_EDGE('',*,*,#2380,.F.);
#3151=ORIENTED_EDGE('',*,*,#2381,.F.);
#3152=ORIENTED_EDGE('',*,*,#2382,.T.);
#3153=ORIENTED_EDGE('',*,*,#2380,.T.);
#3154=ORIENTED_EDGE('',*,*,#2382,.F.);
#3155=ORIENTED_EDGE('',*,*,#2383,.F.);
#3156=ORIENTED_EDGE('',*,*,#2384,.T.);
#3157=ORIENTED_EDGE('',*,*,#2381,.T.);
#3158=ORIENTED_EDGE('',*,*,#2384,.F.);
#3159=ORIENTED_EDGE('',*,*,#2385,.F.);
#3160=ORIENTED_EDGE('',*,*,#2386,.T.);
#3161=ORIENTED_EDGE('',*,*,#2383,.T.);
#3162=ORIENTED_EDGE('',*,*,#2386,.F.);
#3163=ORIENTED_EDGE('',*,*,#2385,.T.);
#3164=ORIENTED_EDGE('',*,*,#2387,.F.);
#3165=ORIENTED_EDGE('',*,*,#2388,.F.);
#3166=ORIENTED_EDGE('',*,*,#2389,.T.);
#3167=ORIENTED_EDGE('',*,*,#2387,.T.);
#3168=ORIENTED_EDGE('',*,*,#2389,.F.);
#3169=ORIENTED_EDGE('',*,*,#2390,.F.);
#3170=ORIENTED_EDGE('',*,*,#2391,.T.);
#3171=ORIENTED_EDGE('',*,*,#2388,.T.);
#3172=ORIENTED_EDGE('',*,*,#2391,.F.);
#3173=ORIENTED_EDGE('',*,*,#2392,.F.);
#3174=ORIENTED_EDGE('',*,*,#2393,.T.);
#3175=ORIENTED_EDGE('',*,*,#2390,.T.);
#3176=ORIENTED_EDGE('',*,*,#2393,.F.);
#3177=ORIENTED_EDGE('',*,*,#2392,.T.);
#3178=ORIENTED_EDGE('',*,*,#2394,.T.);
#3179=ORIENTED_EDGE('',*,*,#2395,.T.);
#3180=ORIENTED_EDGE('',*,*,#2396,.T.);
#3181=ORIENTED_EDGE('',*,*,#2397,.F.);
#3182=ORIENTED_EDGE('',*,*,#2398,.T.);
#3183=ORIENTED_EDGE('',*,*,#2399,.T.);
#3184=ORIENTED_EDGE('',*,*,#2400,.T.);
#3185=ORIENTED_EDGE('',*,*,#2395,.F.);
#3186=ORIENTED_EDGE('',*,*,#2401,.T.);
#3187=ORIENTED_EDGE('',*,*,#2402,.T.);
#3188=ORIENTED_EDGE('',*,*,#2403,.T.);
#3189=ORIENTED_EDGE('',*,*,#2399,.F.);
#3190=ORIENTED_EDGE('',*,*,#2404,.T.);
#3191=ORIENTED_EDGE('',*,*,#2405,.T.);
#3192=ORIENTED_EDGE('',*,*,#2406,.T.);
#3193=ORIENTED_EDGE('',*,*,#2402,.F.);
#3194=ORIENTED_EDGE('',*,*,#2407,.T.);
#3195=ORIENTED_EDGE('',*,*,#2408,.T.);
#3196=ORIENTED_EDGE('',*,*,#2409,.T.);
#3197=ORIENTED_EDGE('',*,*,#2405,.F.);
#3198=ORIENTED_EDGE('',*,*,#2410,.T.);
#3199=ORIENTED_EDGE('',*,*,#2397,.T.);
#3200=ORIENTED_EDGE('',*,*,#2411,.T.);
#3201=ORIENTED_EDGE('',*,*,#2408,.F.);
#3202=ORIENTED_EDGE('',*,*,#2410,.F.);
#3203=ORIENTED_EDGE('',*,*,#2407,.F.);
#3204=ORIENTED_EDGE('',*,*,#2404,.F.);
#3205=ORIENTED_EDGE('',*,*,#2401,.F.);
#3206=ORIENTED_EDGE('',*,*,#2398,.F.);
#3207=ORIENTED_EDGE('',*,*,#2394,.F.);
#3208=ORIENTED_EDGE('',*,*,#2411,.F.);
#3209=ORIENTED_EDGE('',*,*,#2396,.F.);
#3210=ORIENTED_EDGE('',*,*,#2400,.F.);
#3211=ORIENTED_EDGE('',*,*,#2403,.F.);
#3212=ORIENTED_EDGE('',*,*,#2406,.F.);
#3213=ORIENTED_EDGE('',*,*,#2409,.F.);
#3214=ORIENTED_EDGE('',*,*,#2412,.F.);
#3215=ORIENTED_EDGE('',*,*,#2413,.F.);
#3216=ORIENTED_EDGE('',*,*,#2414,.T.);
#3217=ORIENTED_EDGE('',*,*,#2412,.T.);
#3218=ORIENTED_EDGE('',*,*,#2414,.F.);
#3219=ORIENTED_EDGE('',*,*,#2415,.F.);
#3220=ORIENTED_EDGE('',*,*,#2416,.T.);
#3221=ORIENTED_EDGE('',*,*,#2413,.T.);
#3222=ORIENTED_EDGE('',*,*,#2416,.F.);
#3223=ORIENTED_EDGE('',*,*,#2417,.F.);
#3224=ORIENTED_EDGE('',*,*,#2418,.T.);
#3225=ORIENTED_EDGE('',*,*,#2415,.T.);
#3226=ORIENTED_EDGE('',*,*,#2418,.F.);
#3227=ORIENTED_EDGE('',*,*,#2417,.T.);
#3228=ORIENTED_EDGE('',*,*,#2419,.F.);
#3229=ORIENTED_EDGE('',*,*,#2420,.F.);
#3230=ORIENTED_EDGE('',*,*,#2421,.T.);
#3231=ORIENTED_EDGE('',*,*,#2419,.T.);
#3232=ORIENTED_EDGE('',*,*,#2421,.F.);
#3233=ORIENTED_EDGE('',*,*,#2422,.F.);
#3234=ORIENTED_EDGE('',*,*,#2423,.T.);
#3235=ORIENTED_EDGE('',*,*,#2420,.T.);
#3236=ORIENTED_EDGE('',*,*,#2423,.F.);
#3237=ORIENTED_EDGE('',*,*,#2424,.F.);
#3238=ORIENTED_EDGE('',*,*,#2425,.T.);
#3239=ORIENTED_EDGE('',*,*,#2422,.T.);
#3240=ORIENTED_EDGE('',*,*,#2425,.F.);
#3241=ORIENTED_EDGE('',*,*,#2424,.T.);
#3242=ORIENTED_EDGE('',*,*,#2426,.T.);
#3243=ORIENTED_EDGE('',*,*,#2427,.T.);
#3244=ORIENTED_EDGE('',*,*,#2428,.T.);
#3245=ORIENTED_EDGE('',*,*,#2429,.F.);
#3246=ORIENTED_EDGE('',*,*,#2430,.T.);
#3247=ORIENTED_EDGE('',*,*,#2431,.T.);
#3248=ORIENTED_EDGE('',*,*,#2432,.T.);
#3249=ORIENTED_EDGE('',*,*,#2427,.F.);
#3250=ORIENTED_EDGE('',*,*,#2433,.T.);
#3251=ORIENTED_EDGE('',*,*,#2434,.T.);
#3252=ORIENTED_EDGE('',*,*,#2435,.T.);
#3253=ORIENTED_EDGE('',*,*,#2431,.F.);
#3254=ORIENTED_EDGE('',*,*,#2436,.T.);
#3255=ORIENTED_EDGE('',*,*,#2437,.T.);
#3256=ORIENTED_EDGE('',*,*,#2438,.T.);
#3257=ORIENTED_EDGE('',*,*,#2434,.F.);
#3258=ORIENTED_EDGE('',*,*,#2439,.T.);
#3259=ORIENTED_EDGE('',*,*,#2440,.T.);
#3260=ORIENTED_EDGE('',*,*,#2441,.T.);
#3261=ORIENTED_EDGE('',*,*,#2437,.F.);
#3262=ORIENTED_EDGE('',*,*,#2442,.T.);
#3263=ORIENTED_EDGE('',*,*,#2429,.T.);
#3264=ORIENTED_EDGE('',*,*,#2443,.T.);
#3265=ORIENTED_EDGE('',*,*,#2440,.F.);
#3266=ORIENTED_EDGE('',*,*,#2442,.F.);
#3267=ORIENTED_EDGE('',*,*,#2439,.F.);
#3268=ORIENTED_EDGE('',*,*,#2436,.F.);
#3269=ORIENTED_EDGE('',*,*,#2433,.F.);
#3270=ORIENTED_EDGE('',*,*,#2430,.F.);
#3271=ORIENTED_EDGE('',*,*,#2426,.F.);
#3272=ORIENTED_EDGE('',*,*,#2443,.F.);
#3273=ORIENTED_EDGE('',*,*,#2428,.F.);
#3274=ORIENTED_EDGE('',*,*,#2432,.F.);
#3275=ORIENTED_EDGE('',*,*,#2435,.F.);
#3276=ORIENTED_EDGE('',*,*,#2438,.F.);
#3277=ORIENTED_EDGE('',*,*,#2441,.F.);
#3278=ORIENTED_EDGE('',*,*,#2444,.F.);
#3279=ORIENTED_EDGE('',*,*,#2445,.T.);
#3280=ORIENTED_EDGE('',*,*,#2446,.T.);
#3281=ORIENTED_EDGE('',*,*,#2445,.F.);
#3282=ORIENTED_EDGE('',*,*,#2447,.F.);
#3283=ORIENTED_EDGE('',*,*,#2448,.T.);
#3284=ORIENTED_EDGE('',*,*,#2449,.T.);
#3285=ORIENTED_EDGE('',*,*,#2448,.F.);
#3286=ORIENTED_EDGE('',*,*,#2447,.T.);
#3287=ORIENTED_EDGE('',*,*,#2444,.T.);
#3288=ORIENTED_EDGE('',*,*,#2449,.F.);
#3289=ORIENTED_EDGE('',*,*,#2446,.F.);
#3290=ORIENTED_EDGE('',*,*,#2450,.F.);
#3291=ORIENTED_EDGE('',*,*,#2451,.T.);
#3292=ORIENTED_EDGE('',*,*,#2452,.T.);
#3293=ORIENTED_EDGE('',*,*,#2451,.F.);
#3294=ORIENTED_EDGE('',*,*,#2453,.F.);
#3295=ORIENTED_EDGE('',*,*,#2454,.T.);
#3296=ORIENTED_EDGE('',*,*,#2455,.T.);
#3297=ORIENTED_EDGE('',*,*,#2454,.F.);
#3298=ORIENTED_EDGE('',*,*,#2453,.T.);
#3299=ORIENTED_EDGE('',*,*,#2450,.T.);
#3300=ORIENTED_EDGE('',*,*,#2455,.F.);
#3301=ORIENTED_EDGE('',*,*,#2452,.F.);
#3302=ORIENTED_EDGE('',*,*,#2456,.F.);
#3303=ORIENTED_EDGE('',*,*,#2457,.F.);
#3304=ORIENTED_EDGE('',*,*,#2458,.T.);
#3305=ORIENTED_EDGE('',*,*,#2456,.T.);
#3306=ORIENTED_EDGE('',*,*,#2458,.F.);
#3307=ORIENTED_EDGE('',*,*,#2459,.F.);
#3308=ORIENTED_EDGE('',*,*,#2460,.T.);
#3309=ORIENTED_EDGE('',*,*,#2457,.T.);
#3310=ORIENTED_EDGE('',*,*,#2460,.F.);
#3311=ORIENTED_EDGE('',*,*,#2461,.F.);
#3312=ORIENTED_EDGE('',*,*,#2462,.T.);
#3313=ORIENTED_EDGE('',*,*,#2459,.T.);
#3314=ORIENTED_EDGE('',*,*,#2462,.F.);
#3315=ORIENTED_EDGE('',*,*,#2461,.T.);
#3316=ORIENTED_EDGE('',*,*,#2463,.F.);
#3317=ORIENTED_EDGE('',*,*,#2464,.F.);
#3318=ORIENTED_EDGE('',*,*,#2465,.T.);
#3319=ORIENTED_EDGE('',*,*,#2463,.T.);
#3320=ORIENTED_EDGE('',*,*,#2465,.F.);
#3321=ORIENTED_EDGE('',*,*,#2466,.F.);
#3322=ORIENTED_EDGE('',*,*,#2467,.T.);
#3323=ORIENTED_EDGE('',*,*,#2464,.T.);
#3324=ORIENTED_EDGE('',*,*,#2467,.F.);
#3325=ORIENTED_EDGE('',*,*,#2468,.F.);
#3326=ORIENTED_EDGE('',*,*,#2469,.T.);
#3327=ORIENTED_EDGE('',*,*,#2466,.T.);
#3328=ORIENTED_EDGE('',*,*,#2469,.F.);
#3329=ORIENTED_EDGE('',*,*,#2468,.T.);
#3330=ORIENTED_EDGE('',*,*,#2470,.T.);
#3331=ORIENTED_EDGE('',*,*,#2471,.T.);
#3332=ORIENTED_EDGE('',*,*,#2472,.T.);
#3333=ORIENTED_EDGE('',*,*,#2473,.F.);
#3334=ORIENTED_EDGE('',*,*,#2474,.T.);
#3335=ORIENTED_EDGE('',*,*,#2475,.T.);
#3336=ORIENTED_EDGE('',*,*,#2476,.T.);
#3337=ORIENTED_EDGE('',*,*,#2471,.F.);
#3338=ORIENTED_EDGE('',*,*,#2477,.T.);
#3339=ORIENTED_EDGE('',*,*,#2478,.T.);
#3340=ORIENTED_EDGE('',*,*,#2479,.T.);
#3341=ORIENTED_EDGE('',*,*,#2475,.F.);
#3342=ORIENTED_EDGE('',*,*,#2480,.T.);
#3343=ORIENTED_EDGE('',*,*,#2481,.T.);
#3344=ORIENTED_EDGE('',*,*,#2482,.T.);
#3345=ORIENTED_EDGE('',*,*,#2478,.F.);
#3346=ORIENTED_EDGE('',*,*,#2483,.T.);
#3347=ORIENTED_EDGE('',*,*,#2484,.T.);
#3348=ORIENTED_EDGE('',*,*,#2485,.T.);
#3349=ORIENTED_EDGE('',*,*,#2481,.F.);
#3350=ORIENTED_EDGE('',*,*,#2486,.T.);
#3351=ORIENTED_EDGE('',*,*,#2473,.T.);
#3352=ORIENTED_EDGE('',*,*,#2487,.T.);
#3353=ORIENTED_EDGE('',*,*,#2484,.F.);
#3354=ORIENTED_EDGE('',*,*,#2486,.F.);
#3355=ORIENTED_EDGE('',*,*,#2483,.F.);
#3356=ORIENTED_EDGE('',*,*,#2480,.F.);
#3357=ORIENTED_EDGE('',*,*,#2477,.F.);
#3358=ORIENTED_EDGE('',*,*,#2474,.F.);
#3359=ORIENTED_EDGE('',*,*,#2470,.F.);
#3360=ORIENTED_EDGE('',*,*,#2487,.F.);
#3361=ORIENTED_EDGE('',*,*,#2472,.F.);
#3362=ORIENTED_EDGE('',*,*,#2476,.F.);
#3363=ORIENTED_EDGE('',*,*,#2479,.F.);
#3364=ORIENTED_EDGE('',*,*,#2482,.F.);
#3365=ORIENTED_EDGE('',*,*,#2485,.F.);
#3366=CYLINDRICAL_SURFACE('',#3838,0.210000000000001);
#3367=CYLINDRICAL_SURFACE('',#3841,0.21);
#3368=CYLINDRICAL_SURFACE('',#3844,0.21);
#3369=CYLINDRICAL_SURFACE('',#3847,0.210000000000001);
#3370=CYLINDRICAL_SURFACE('',#3850,0.210000000000001);
#3371=CYLINDRICAL_SURFACE('',#3853,0.210000000000001);
#3372=CYLINDRICAL_SURFACE('',#3856,0.21);
#3373=CYLINDRICAL_SURFACE('',#3859,0.21);
#3374=CYLINDRICAL_SURFACE('',#3862,0.21);
#3375=CYLINDRICAL_SURFACE('',#3865,0.21);
#3376=CYLINDRICAL_SURFACE('',#3868,0.210000000000001);
#3377=CYLINDRICAL_SURFACE('',#3871,0.210000000000001);
#3378=CYLINDRICAL_SURFACE('',#3884,0.6);
#3379=CYLINDRICAL_SURFACE('',#3893,0.525);
#3380=CYLINDRICAL_SURFACE('',#3895,0.525);
#3381=CYLINDRICAL_SURFACE('',#3905,0.225);
#3382=CYLINDRICAL_SURFACE('',#3908,0.165);
#3383=CYLINDRICAL_SURFACE('',#3910,0.275);
#3384=CYLINDRICAL_SURFACE('',#3912,0.275);
#3385=CYLINDRICAL_SURFACE('',#3914,0.6);
#3386=CYLINDRICAL_SURFACE('',#3943,0.425);
#3387=CYLINDRICAL_SURFACE('',#3951,0.24505);
#3388=CYLINDRICAL_SURFACE('',#3953,0.475);
#3389=CYLINDRICAL_SURFACE('',#3958,0.475);
#3390=CYLINDRICAL_SURFACE('',#3963,0.275);
#3391=CYLINDRICAL_SURFACE('',#3965,0.275);
#3392=CYLINDRICAL_SURFACE('',#3982,0.165);
#3393=CYLINDRICAL_SURFACE('',#3985,0.165);
#3394=CYLINDRICAL_SURFACE('',#3988,0.165);
#3395=CYLINDRICAL_SURFACE('',#3991,0.165);
#3396=CYLINDRICAL_SURFACE('',#3994,0.210000000000001);
#3397=CYLINDRICAL_SURFACE('',#3998,0.210000000000001);
#3398=CYLINDRICAL_SURFACE('',#4002,0.210000000000001);
#3399=CYLINDRICAL_SURFACE('',#4006,0.210000000000001);
#3400=CYLINDRICAL_SURFACE('',#4010,1.05);
#3401=CYLINDRICAL_SURFACE('',#4013,1.05);
#3402=CYLINDRICAL_SURFACE('',#4023,0.25);
#3403=CYLINDRICAL_SURFACE('',#4026,0.274999999999999);
#3404=CYLINDRICAL_SURFACE('',#4029,0.275);
#3405=CYLINDRICAL_SURFACE('',#4032,0.275);
#3406=CYLINDRICAL_SURFACE('',#4035,0.274999999999999);
#3407=CYLINDRICAL_SURFACE('',#4056,1.05);
#3408=CYLINDRICAL_SURFACE('',#4060,1.);
#3409=CYLINDRICAL_SURFACE('',#4064,1.05);
#3410=CYLINDRICAL_SURFACE('',#4068,1.);
#3411=CYLINDRICAL_SURFACE('',#4072,1.05);
#3412=CYLINDRICAL_SURFACE('',#4076,0.9);
#3413=CYLINDRICAL_SURFACE('',#4089,0.895);
#3414=CYLINDRICAL_SURFACE('',#4093,0.605);
#3415=CYLINDRICAL_SURFACE('',#4097,0.225);
#3416=CYLINDRICAL_SURFACE('',#4100,0.225);
#3417=CYLINDRICAL_SURFACE('',#4103,0.225);
#3418=CYLINDRICAL_SURFACE('',#4106,0.225);
#3419=CYLINDRICAL_SURFACE('',#4109,0.7);
#3420=CYLINDRICAL_SURFACE('',#4112,0.7);
#3421=CYLINDRICAL_SURFACE('',#4126,0.35);
#3422=CYLINDRICAL_SURFACE('',#4134,0.1954);
#3423=CYLINDRICAL_SURFACE('',#4152,0.425);
#3424=CYLINDRICAL_SURFACE('',#4160,0.24505);
#3425=CYLINDRICAL_SURFACE('',#4201,0.33);
#3426=CYLINDRICAL_SURFACE('',#4204,1.5);
#3427=CYLINDRICAL_SURFACE('',#4210,0.32);
#3428=CYLINDRICAL_SURFACE('',#4213,0.6);
#3429=CYLINDRICAL_SURFACE('',#4223,0.5);
#3430=CYLINDRICAL_SURFACE('',#4231,0.2942);
#3431=ADVANCED_FACE('',(#526),#3366,.F.);
#3432=ADVANCED_FACE('',(#527),#3367,.F.);
#3433=ADVANCED_FACE('',(#528),#3368,.F.);
#3434=ADVANCED_FACE('',(#529),#3369,.F.);
#3435=ADVANCED_FACE('',(#530),#3370,.F.);
#3436=ADVANCED_FACE('',(#531),#3371,.F.);
#3437=ADVANCED_FACE('',(#532),#3372,.F.);
#3438=ADVANCED_FACE('',(#533),#3373,.F.);
#3439=ADVANCED_FACE('',(#534),#3374,.F.);
#3440=ADVANCED_FACE('',(#535),#3375,.F.);
#3441=ADVANCED_FACE('',(#536),#3376,.F.);
#3442=ADVANCED_FACE('',(#537),#3377,.F.);
#3443=ADVANCED_FACE('',(#538),#401,.T.);
#3444=ADVANCED_FACE('',(#539),#402,.T.);
#3445=ADVANCED_FACE('',(#540),#403,.T.);
#3446=ADVANCED_FACE('',(#541),#404,.T.);
#3447=ADVANCED_FACE('',(#542,#304,#305,#306,#307,#308,#309,#310,#311,#312,
#313,#314,#315),#405,.T.);
#3448=ADVANCED_FACE('',(#543,#316,#317,#318,#319,#320,#321,#322,#323,#324,
#325,#326,#327),#406,.F.);
#3449=ADVANCED_FACE('',(#544),#227,.T.);
#3450=ADVANCED_FACE('',(#545),#3378,.T.);
#3451=ADVANCED_FACE('',(#546),#407,.F.);
#3452=ADVANCED_FACE('',(#547),#228,.T.);
#3453=ADVANCED_FACE('',(#548),#408,.T.);
#3454=ADVANCED_FACE('',(#549),#409,.F.);
#3455=ADVANCED_FACE('',(#550),#3379,.F.);
#3456=ADVANCED_FACE('',(#551),#3380,.F.);
#3457=ADVANCED_FACE('',(#552),#410,.F.);
#3458=ADVANCED_FACE('',(#553,#328),#411,.T.);
#3459=ADVANCED_FACE('',(#554,#329),#412,.T.);
#3460=ADVANCED_FACE('',(#555,#330),#413,.T.);
#3461=ADVANCED_FACE('',(#556),#3381,.F.);
#3462=ADVANCED_FACE('',(#557),#3382,.F.);
#3463=ADVANCED_FACE('',(#558),#3383,.F.);
#3464=ADVANCED_FACE('',(#559),#3384,.F.);
#3465=ADVANCED_FACE('',(#560),#3385,.F.);
#3466=ADVANCED_FACE('',(#561,#331),#414,.T.);
#3467=ADVANCED_FACE('',(#562),#415,.T.);
#3468=ADVANCED_FACE('',(#563,#332,#333),#416,.T.);
#3469=ADVANCED_FACE('',(#564),#417,.T.);
#3470=ADVANCED_FACE('',(#565,#334),#418,.T.);
#3471=ADVANCED_FACE('',(#566),#419,.T.);
#3472=ADVANCED_FACE('',(#567,#335),#420,.T.);
#3473=ADVANCED_FACE('',(#568),#421,.T.);
#3474=ADVANCED_FACE('',(#569,#336),#422,.T.);
#3475=ADVANCED_FACE('',(#570),#423,.T.);
#3476=ADVANCED_FACE('',(#571,#337),#424,.T.);
#3477=ADVANCED_FACE('',(#572),#425,.F.);
#3478=ADVANCED_FACE('',(#573),#426,.F.);
#3479=ADVANCED_FACE('',(#574),#427,.F.);
#3480=ADVANCED_FACE('',(#575),#428,.F.);
#3481=ADVANCED_FACE('',(#576),#429,.F.);
#3482=ADVANCED_FACE('',(#577),#430,.F.);
#3483=ADVANCED_FACE('',(#578),#431,.F.);
#3484=ADVANCED_FACE('',(#579),#432,.F.);
#3485=ADVANCED_FACE('',(#580),#433,.F.);
#3486=ADVANCED_FACE('',(#581),#434,.T.);
#3487=ADVANCED_FACE('',(#582),#229,.T.);
#3488=ADVANCED_FACE('',(#583),#3386,.T.);
#3489=ADVANCED_FACE('',(#584),#230,.T.);
#3490=ADVANCED_FACE('',(#585,#338),#435,.T.);
#3491=ADVANCED_FACE('',(#586),#231,.T.);
#3492=ADVANCED_FACE('',(#587),#3387,.T.);
#3493=ADVANCED_FACE('',(#588),#3388,.F.);
#3494=ADVANCED_FACE('',(#589,#339),#436,.T.);
#3495=ADVANCED_FACE('',(#590),#3389,.F.);
#3496=ADVANCED_FACE('',(#591,#340),#437,.T.);
#3497=ADVANCED_FACE('',(#592),#3390,.F.);
#3498=ADVANCED_FACE('',(#593),#3391,.F.);
#3499=ADVANCED_FACE('',(#594),#438,.T.);
#3500=ADVANCED_FACE('',(#595),#439,.T.);
#3501=ADVANCED_FACE('',(#596),#440,.T.);
#3502=ADVANCED_FACE('',(#597),#441,.T.);
#3503=ADVANCED_FACE('',(#598,#341,#342),#442,.T.);
#3504=ADVANCED_FACE('',(#599,#343,#344),#443,.F.);
#3505=ADVANCED_FACE('',(#600),#444,.T.);
#3506=ADVANCED_FACE('',(#601),#445,.T.);
#3507=ADVANCED_FACE('',(#602),#446,.T.);
#3508=ADVANCED_FACE('',(#603),#447,.T.);
#3509=ADVANCED_FACE('',(#604),#448,.T.);
#3510=ADVANCED_FACE('',(#605),#449,.F.);
#3511=ADVANCED_FACE('',(#606),#3392,.F.);
#3512=ADVANCED_FACE('',(#607),#3393,.F.);
#3513=ADVANCED_FACE('',(#608),#3394,.F.);
#3514=ADVANCED_FACE('',(#609),#3395,.F.);
#3515=ADVANCED_FACE('',(#610),#3396,.F.);
#3516=ADVANCED_FACE('',(#611),#450,.T.);
#3517=ADVANCED_FACE('',(#612),#3397,.F.);
#3518=ADVANCED_FACE('',(#613),#451,.T.);
#3519=ADVANCED_FACE('',(#614),#3398,.F.);
#3520=ADVANCED_FACE('',(#615),#452,.T.);
#3521=ADVANCED_FACE('',(#616),#3399,.F.);
#3522=ADVANCED_FACE('',(#617),#453,.T.);
#3523=ADVANCED_FACE('',(#618),#3400,.F.);
#3524=ADVANCED_FACE('',(#619),#3401,.F.);
#3525=ADVANCED_FACE('',(#620),#454,.T.);
#3526=ADVANCED_FACE('',(#621,#345,#346,#347,#348,#349,#350),#455,.T.);
#3527=ADVANCED_FACE('',(#622),#456,.T.);
#3528=ADVANCED_FACE('',(#623,#351,#352,#353,#354,#355,#356),#457,.T.);
#3529=ADVANCED_FACE('',(#624,#357,#358,#359,#360),#458,.T.);
#3530=ADVANCED_FACE('',(#625),#459,.F.);
#3531=ADVANCED_FACE('',(#626),#3402,.F.);
#3532=ADVANCED_FACE('',(#627),#3403,.F.);
#3533=ADVANCED_FACE('',(#628),#3404,.F.);
#3534=ADVANCED_FACE('',(#629),#3405,.F.);
#3535=ADVANCED_FACE('',(#630),#3406,.F.);
#3536=ADVANCED_FACE('',(#631),#460,.T.);
#3537=ADVANCED_FACE('',(#632),#461,.T.);
#3538=ADVANCED_FACE('',(#633),#462,.T.);
#3539=ADVANCED_FACE('',(#634),#463,.T.);
#3540=ADVANCED_FACE('',(#635,#361,#362,#363,#364,#365),#464,.T.);
#3541=ADVANCED_FACE('',(#636,#366,#367,#368,#369,#370),#465,.F.);
#3542=ADVANCED_FACE('',(#637),#466,.F.);
#3543=ADVANCED_FACE('',(#638),#467,.F.);
#3544=ADVANCED_FACE('',(#639),#468,.F.);
#3545=ADVANCED_FACE('',(#640),#469,.F.);
#3546=ADVANCED_FACE('',(#641),#470,.F.);
#3547=ADVANCED_FACE('',(#642,#371),#471,.T.);
#3548=ADVANCED_FACE('',(#643),#3407,.T.);
#3549=ADVANCED_FACE('',(#644,#372),#472,.T.);
#3550=ADVANCED_FACE('',(#645),#3408,.T.);
#3551=ADVANCED_FACE('',(#646,#373),#473,.T.);
#3552=ADVANCED_FACE('',(#647),#3409,.T.);
#3553=ADVANCED_FACE('',(#648,#374),#474,.T.);
#3554=ADVANCED_FACE('',(#649),#3410,.T.);
#3555=ADVANCED_FACE('',(#650,#375),#475,.T.);
#3556=ADVANCED_FACE('',(#651),#3411,.T.);
#3557=ADVANCED_FACE('',(#652,#376),#476,.T.);
#3558=ADVANCED_FACE('',(#653,#377),#3412,.F.);
#3559=ADVANCED_FACE('',(#654),#477,.F.);
#3560=ADVANCED_FACE('',(#655),#478,.F.);
#3561=ADVANCED_FACE('',(#656),#479,.F.);
#3562=ADVANCED_FACE('',(#657),#480,.F.);
#3563=ADVANCED_FACE('',(#658,#378),#481,.T.);
#3564=ADVANCED_FACE('',(#659,#379),#3413,.T.);
#3565=ADVANCED_FACE('',(#660,#380),#482,.T.);
#3566=ADVANCED_FACE('',(#661,#381),#3414,.F.);
#3567=ADVANCED_FACE('',(#662),#3415,.F.);
#3568=ADVANCED_FACE('',(#663),#3416,.F.);
#3569=ADVANCED_FACE('',(#664),#3417,.F.);
#3570=ADVANCED_FACE('',(#665),#3418,.F.);
#3571=ADVANCED_FACE('',(#666),#3419,.F.);
#3572=ADVANCED_FACE('',(#667),#3420,.F.);
#3573=ADVANCED_FACE('',(#668),#483,.T.);
#3574=ADVANCED_FACE('',(#669,#382,#383,#384,#385,#386,#387),#484,.T.);
#3575=ADVANCED_FACE('',(#670),#485,.T.);
#3576=ADVANCED_FACE('',(#671,#388,#389,#390,#391,#392,#393),#486,.T.);
#3577=ADVANCED_FACE('',(#672),#487,.T.);
#3578=ADVANCED_FACE('',(#673),#488,.F.);
#3579=ADVANCED_FACE('',(#674),#489,.T.);
#3580=ADVANCED_FACE('',(#675),#232,.T.);
#3581=ADVANCED_FACE('',(#676),#3421,.T.);
#3582=ADVANCED_FACE('',(#677),#233,.T.);
#3583=ADVANCED_FACE('',(#678,#394),#490,.T.);
#3584=ADVANCED_FACE('',(#679),#234,.T.);
#3585=ADVANCED_FACE('',(#680),#3422,.T.);
#3586=ADVANCED_FACE('',(#681),#235,.T.);
#3587=ADVANCED_FACE('',(#682),#491,.T.);
#3588=ADVANCED_FACE('',(#683),#492,.F.);
#3589=ADVANCED_FACE('',(#684),#493,.F.);
#3590=ADVANCED_FACE('',(#685),#494,.F.);
#3591=ADVANCED_FACE('',(#686),#495,.F.);
#3592=ADVANCED_FACE('',(#687),#496,.F.);
#3593=ADVANCED_FACE('',(#688),#497,.F.);
#3594=ADVANCED_FACE('',(#689),#498,.F.);
#3595=ADVANCED_FACE('',(#690),#499,.F.);
#3596=ADVANCED_FACE('',(#691),#500,.T.);
#3597=ADVANCED_FACE('',(#692),#236,.T.);
#3598=ADVANCED_FACE('',(#693),#3423,.T.);
#3599=ADVANCED_FACE('',(#694),#237,.T.);
#3600=ADVANCED_FACE('',(#695,#395),#501,.T.);
#3601=ADVANCED_FACE('',(#696),#238,.T.);
#3602=ADVANCED_FACE('',(#697),#3424,.T.);
#3603=ADVANCED_FACE('',(#698),#239,.T.);
#3604=ADVANCED_FACE('',(#699),#502,.T.);
#3605=ADVANCED_FACE('',(#700),#503,.F.);
#3606=ADVANCED_FACE('',(#701),#504,.F.);
#3607=ADVANCED_FACE('',(#702),#505,.F.);
#3608=ADVANCED_FACE('',(#703),#506,.F.);
#3609=ADVANCED_FACE('',(#704),#507,.F.);
#3610=ADVANCED_FACE('',(#705),#508,.F.);
#3611=ADVANCED_FACE('',(#706),#509,.F.);
#3612=ADVANCED_FACE('',(#707),#510,.F.);
#3613=ADVANCED_FACE('',(#708),#3425,.F.);
#3614=ADVANCED_FACE('',(#709),#3426,.T.);
#3615=ADVANCED_FACE('',(#710,#396),#511,.T.);
#3616=ADVANCED_FACE('',(#711,#397),#512,.F.);
#3617=ADVANCED_FACE('',(#712),#3427,.F.);
#3618=ADVANCED_FACE('',(#713),#3428,.T.);
#3619=ADVANCED_FACE('',(#714,#398),#513,.T.);
#3620=ADVANCED_FACE('',(#715,#399),#514,.F.);
#3621=ADVANCED_FACE('',(#716),#515,.T.);
#3622=ADVANCED_FACE('',(#717),#240,.T.);
#3623=ADVANCED_FACE('',(#718),#3429,.T.);
#3624=ADVANCED_FACE('',(#719),#241,.T.);
#3625=ADVANCED_FACE('',(#720,#400),#516,.T.);
#3626=ADVANCED_FACE('',(#721),#242,.T.);
#3627=ADVANCED_FACE('',(#722),#3430,.T.);
#3628=ADVANCED_FACE('',(#723),#243,.T.);
#3629=ADVANCED_FACE('',(#724),#517,.T.);
#3630=ADVANCED_FACE('',(#725),#518,.F.);
#3631=ADVANCED_FACE('',(#726),#519,.F.);
#3632=ADVANCED_FACE('',(#727),#520,.F.);
#3633=ADVANCED_FACE('',(#728),#521,.F.);
#3634=ADVANCED_FACE('',(#729),#522,.F.);
#3635=ADVANCED_FACE('',(#730),#523,.F.);
#3636=ADVANCED_FACE('',(#731),#524,.F.);
#3637=ADVANCED_FACE('',(#732),#525,.F.);
#3638=CLOSED_SHELL('',(#3431,#3432,#3433,#3434,#3435,#3436,#3437,#3438,
#3439,#3440,#3441,#3442,#3443,#3444,#3445,#3446,#3447,#3448));
#3639=CLOSED_SHELL('',(#3449,#3450,#3451,#3452,#3453));
#3640=CLOSED_SHELL('',(#3454,#3455,#3456,#3457,#3458,#3459,#3460,#3461,
#3462,#3463,#3464,#3465,#3466,#3467,#3468,#3469,#3470,#3471,#3472,#3473,
#3474,#3475,#3476));
#3641=CLOSED_SHELL('',(#3477,#3478,#3479,#3480,#3481,#3482,#3483,#3484));
#3642=CLOSED_SHELL('',(#3485,#3486,#3487,#3488,#3489,#3490,#3491,#3492));
#3643=CLOSED_SHELL('',(#3493,#3494,#3495,#3496,#3497,#3498,#3499,#3500,
#3501,#3502,#3503,#3504));
#3644=CLOSED_SHELL('',(#3505,#3506,#3507,#3508,#3509,#3510));
#3645=CLOSED_SHELL('',(#3511,#3512,#3513,#3514,#3515,#3516,#3517,#3518,
#3519,#3520,#3521,#3522,#3523,#3524,#3525,#3526,#3527,#3528,#3529,#3530));
#3646=CLOSED_SHELL('',(#3531,#3532,#3533,#3534,#3535,#3536,#3537,#3538,
#3539,#3540,#3541));
#3647=CLOSED_SHELL('',(#3542,#3543,#3544,#3545,#3546,#3547,#3548,#3549,
#3550,#3551,#3552,#3553,#3554,#3555,#3556,#3557,#3558));
#3648=CLOSED_SHELL('',(#3559,#3560,#3561,#3562,#3563,#3564,#3565,#3566));
#3649=CLOSED_SHELL('',(#3567,#3568,#3569,#3570,#3571,#3572,#3573,#3574,
#3575,#3576,#3577,#3578));
#3650=CLOSED_SHELL('',(#3579,#3580,#3581,#3582,#3583,#3584,#3585,#3586,
#3587));
#3651=CLOSED_SHELL('',(#3588,#3589,#3590,#3591,#3592,#3593,#3594,#3595));
#3652=CLOSED_SHELL('',(#3596,#3597,#3598,#3599,#3600,#3601,#3602,#3603,
#3604));
#3653=CLOSED_SHELL('',(#3605,#3606,#3607,#3608,#3609,#3610,#3611,#3612));
#3654=CLOSED_SHELL('',(#3613,#3614,#3615,#3616));
#3655=CLOSED_SHELL('',(#3617,#3618,#3619,#3620));
#3656=CLOSED_SHELL('',(#3621,#3622,#3623,#3624,#3625,#3626,#3627,#3628,
#3629));
#3657=CLOSED_SHELL('',(#3630,#3631,#3632,#3633,#3634,#3635,#3636,#3637));
#3658=DERIVED_UNIT_ELEMENT(#3690,1.);
#3659=DERIVED_UNIT_ELEMENT(#6465,-3.);
#3660=DERIVED_UNIT_ELEMENT(#3690,1.);
#3661=DERIVED_UNIT_ELEMENT(#6465,-3.);
#3662=DERIVED_UNIT_ELEMENT(#3690,1.);
#3663=DERIVED_UNIT_ELEMENT(#6465,-3.);
#3664=DERIVED_UNIT_ELEMENT(#3690,1.);
#3665=DERIVED_UNIT_ELEMENT(#6465,-3.);
#3666=DERIVED_UNIT_ELEMENT(#3690,1.);
#3667=DERIVED_UNIT_ELEMENT(#6465,-3.);
#3668=DERIVED_UNIT_ELEMENT(#3690,1.);
#3669=DERIVED_UNIT_ELEMENT(#6465,-3.);
#3670=DERIVED_UNIT_ELEMENT(#3690,1.);
#3671=DERIVED_UNIT_ELEMENT(#6465,-3.);
#3672=DERIVED_UNIT_ELEMENT(#3690,1.);
#3673=DERIVED_UNIT_ELEMENT(#6465,-3.);
#3674=DERIVED_UNIT_ELEMENT(#3690,1.);
#3675=DERIVED_UNIT_ELEMENT(#6465,-3.);
#3676=DERIVED_UNIT_ELEMENT(#3690,1.);
#3677=DERIVED_UNIT_ELEMENT(#6465,-3.);
#3678=DERIVED_UNIT_ELEMENT(#3690,1.);
#3679=DERIVED_UNIT_ELEMENT(#6465,-3.);
#3680=DERIVED_UNIT_ELEMENT(#3690,1.);
#3681=DERIVED_UNIT_ELEMENT(#6465,-3.);
#3682=DERIVED_UNIT_ELEMENT(#3690,1.);
#3683=DERIVED_UNIT_ELEMENT(#6465,-3.);
#3684=DERIVED_UNIT_ELEMENT(#3690,1.);
#3685=DERIVED_UNIT_ELEMENT(#6465,-3.);
#3686=DERIVED_UNIT_ELEMENT(#3690,1.);
#3687=DERIVED_UNIT_ELEMENT(#6465,-3.);
#3688=DERIVED_UNIT_ELEMENT(#3690,1.);
#3689=DERIVED_UNIT_ELEMENT(#6465,-3.);
#3690=(
MASS_UNIT()
NAMED_UNIT(*)
SI_UNIT(.KILO.,.GRAM.)
);
#3691=DERIVED_UNIT((#3658,#3659));
#3692=DERIVED_UNIT((#3660,#3661));
#3693=DERIVED_UNIT((#3662,#3663));
#3694=DERIVED_UNIT((#3664,#3665));
#3695=DERIVED_UNIT((#3666,#3667));
#3696=DERIVED_UNIT((#3668,#3669));
#3697=DERIVED_UNIT((#3670,#3671));
#3698=DERIVED_UNIT((#3672,#3673));
#3699=DERIVED_UNIT((#3674,#3675));
#3700=DERIVED_UNIT((#3676,#3677));
#3701=DERIVED_UNIT((#3678,#3679));
#3702=DERIVED_UNIT((#3680,#3681));
#3703=DERIVED_UNIT((#3682,#3683));
#3704=DERIVED_UNIT((#3684,#3685));
#3705=DERIVED_UNIT((#3686,#3687));
#3706=DERIVED_UNIT((#3688,#3689));
#3707=MEASURE_REPRESENTATION_ITEM('density measure',
POSITIVE_RATIO_MEASURE(7850.),#3691);
#3708=MEASURE_REPRESENTATION_ITEM('density measure',
POSITIVE_RATIO_MEASURE(7850.),#3692);
#3709=MEASURE_REPRESENTATION_ITEM('density measure',
POSITIVE_RATIO_MEASURE(7850.),#3693);
#3710=MEASURE_REPRESENTATION_ITEM('density measure',
POSITIVE_RATIO_MEASURE(7850.),#3694);
#3711=MEASURE_REPRESENTATION_ITEM('density measure',
POSITIVE_RATIO_MEASURE(7850.),#3695);
#3712=MEASURE_REPRESENTATION_ITEM('density measure',
POSITIVE_RATIO_MEASURE(7850.),#3696);
#3713=MEASURE_REPRESENTATION_ITEM('density measure',
POSITIVE_RATIO_MEASURE(7850.),#3697);
#3714=MEASURE_REPRESENTATION_ITEM('density measure',
POSITIVE_RATIO_MEASURE(7850.),#3698);
#3715=MEASURE_REPRESENTATION_ITEM('density measure',
POSITIVE_RATIO_MEASURE(7850.),#3699);
#3716=MEASURE_REPRESENTATION_ITEM('density measure',
POSITIVE_RATIO_MEASURE(7850.),#3700);
#3717=MEASURE_REPRESENTATION_ITEM('density measure',
POSITIVE_RATIO_MEASURE(7850.),#3701);
#3718=MEASURE_REPRESENTATION_ITEM('density measure',
POSITIVE_RATIO_MEASURE(7850.),#3702);
#3719=MEASURE_REPRESENTATION_ITEM('density measure',
POSITIVE_RATIO_MEASURE(7850.),#3703);
#3720=MEASURE_REPRESENTATION_ITEM('density measure',
POSITIVE_RATIO_MEASURE(7850.),#3704);
#3721=MEASURE_REPRESENTATION_ITEM('density measure',
POSITIVE_RATIO_MEASURE(7850.),#3705);
#3722=MEASURE_REPRESENTATION_ITEM('density measure',
POSITIVE_RATIO_MEASURE(7850.),#3706);
#3723=PROPERTY_DEFINITION_REPRESENTATION(#3803,#3755);
#3724=PROPERTY_DEFINITION_REPRESENTATION(#3804,#3756);
#3725=PROPERTY_DEFINITION_REPRESENTATION(#3805,#3757);
#3726=PROPERTY_DEFINITION_REPRESENTATION(#3806,#3758);
#3727=PROPERTY_DEFINITION_REPRESENTATION(#3807,#3759);
#3728=PROPERTY_DEFINITION_REPRESENTATION(#3808,#3760);
#3729=PROPERTY_DEFINITION_REPRESENTATION(#3809,#3761);
#3730=PROPERTY_DEFINITION_REPRESENTATION(#3810,#3762);
#3731=PROPERTY_DEFINITION_REPRESENTATION(#3811,#3763);
#3732=PROPERTY_DEFINITION_REPRESENTATION(#3812,#3764);
#3733=PROPERTY_DEFINITION_REPRESENTATION(#3813,#3765);
#3734=PROPERTY_DEFINITION_REPRESENTATION(#3814,#3766);
#3735=PROPERTY_DEFINITION_REPRESENTATION(#3815,#3767);
#3736=PROPERTY_DEFINITION_REPRESENTATION(#3816,#3768);
#3737=PROPERTY_DEFINITION_REPRESENTATION(#3817,#3769);
#3738=PROPERTY_DEFINITION_REPRESENTATION(#3818,#3770);
#3739=PROPERTY_DEFINITION_REPRESENTATION(#3819,#3771);
#3740=PROPERTY_DEFINITION_REPRESENTATION(#3820,#3772);
#3741=PROPERTY_DEFINITION_REPRESENTATION(#3821,#3773);
#3742=PROPERTY_DEFINITION_REPRESENTATION(#3822,#3774);
#3743=PROPERTY_DEFINITION_REPRESENTATION(#3823,#3775);
#3744=PROPERTY_DEFINITION_REPRESENTATION(#3824,#3776);
#3745=PROPERTY_DEFINITION_REPRESENTATION(#3825,#3777);
#3746=PROPERTY_DEFINITION_REPRESENTATION(#3826,#3778);
#3747=PROPERTY_DEFINITION_REPRESENTATION(#3827,#3779);
#3748=PROPERTY_DEFINITION_REPRESENTATION(#3828,#3780);
#3749=PROPERTY_DEFINITION_REPRESENTATION(#3829,#3781);
#3750=PROPERTY_DEFINITION_REPRESENTATION(#3830,#3782);
#3751=PROPERTY_DEFINITION_REPRESENTATION(#3831,#3783);
#3752=PROPERTY_DEFINITION_REPRESENTATION(#3832,#3784);
#3753=PROPERTY_DEFINITION_REPRESENTATION(#3833,#3785);
#3754=PROPERTY_DEFINITION_REPRESENTATION(#3834,#3786);
#3755=REPRESENTATION('material name',(#3787),#6445);
#3756=REPRESENTATION('density',(#3707),#6445);
#3757=REPRESENTATION('material name',(#3788),#6446);
#3758=REPRESENTATION('density',(#3708),#6446);
#3759=REPRESENTATION('material name',(#3789),#6447);
#3760=REPRESENTATION('density',(#3709),#6447);
#3761=REPRESENTATION('material name',(#3790),#6448);
#3762=REPRESENTATION('density',(#3710),#6448);
#3763=REPRESENTATION('material name',(#3791),#6449);
#3764=REPRESENTATION('density',(#3711),#6449);
#3765=REPRESENTATION('material name',(#3792),#6450);
#3766=REPRESENTATION('density',(#3712),#6450);
#3767=REPRESENTATION('material name',(#3793),#6452);
#3768=REPRESENTATION('density',(#3713),#6452);
#3769=REPRESENTATION('material name',(#3794),#6453);
#3770=REPRESENTATION('density',(#3714),#6453);
#3771=REPRESENTATION('material name',(#3795),#6455);
#3772=REPRESENTATION('density',(#3715),#6455);
#3773=REPRESENTATION('material name',(#3796),#6456);
#3774=REPRESENTATION('density',(#3716),#6456);
#3775=REPRESENTATION('material name',(#3797),#6457);
#3776=REPRESENTATION('density',(#3717),#6457);
#3777=REPRESENTATION('material name',(#3798),#6458);
#3778=REPRESENTATION('density',(#3718),#6458);
#3779=REPRESENTATION('material name',(#3799),#6459);
#3780=REPRESENTATION('density',(#3719),#6459);
#3781=REPRESENTATION('material name',(#3800),#6460);
#3782=REPRESENTATION('density',(#3720),#6460);
#3783=REPRESENTATION('material name',(#3801),#6461);
#3784=REPRESENTATION('density',(#3721),#6461);
#3785=REPRESENTATION('material name',(#3802),#6462);
#3786=REPRESENTATION('density',(#3722),#6462);
#3787=DESCRIPTIVE_REPRESENTATION_ITEM('Steel','Steel');
#3788=DESCRIPTIVE_REPRESENTATION_ITEM('Steel','Steel');
#3789=DESCRIPTIVE_REPRESENTATION_ITEM('Steel','Steel');
#3790=DESCRIPTIVE_REPRESENTATION_ITEM('Steel','Steel');
#3791=DESCRIPTIVE_REPRESENTATION_ITEM('Steel','Steel');
#3792=DESCRIPTIVE_REPRESENTATION_ITEM('Steel','Steel');
#3793=DESCRIPTIVE_REPRESENTATION_ITEM('Steel','Steel');
#3794=DESCRIPTIVE_REPRESENTATION_ITEM('Steel','Steel');
#3795=DESCRIPTIVE_REPRESENTATION_ITEM('Steel','Steel');
#3796=DESCRIPTIVE_REPRESENTATION_ITEM('Steel','Steel');
#3797=DESCRIPTIVE_REPRESENTATION_ITEM('Steel','Steel');
#3798=DESCRIPTIVE_REPRESENTATION_ITEM('Steel','Steel');
#3799=DESCRIPTIVE_REPRESENTATION_ITEM('Steel','Steel');
#3800=DESCRIPTIVE_REPRESENTATION_ITEM('Steel','Steel');
#3801=DESCRIPTIVE_REPRESENTATION_ITEM('Steel','Steel');
#3802=DESCRIPTIVE_REPRESENTATION_ITEM('Steel','Steel');
#3803=PROPERTY_DEFINITION('material property','material name',#6583);
#3804=PROPERTY_DEFINITION('material property','density of part',#6583);
#3805=PROPERTY_DEFINITION('material property','material name',#6584);
#3806=PROPERTY_DEFINITION('material property','density of part',#6584);
#3807=PROPERTY_DEFINITION('material property','material name',#6585);
#3808=PROPERTY_DEFINITION('material property','density of part',#6585);
#3809=PROPERTY_DEFINITION('material property','material name',#6586);
#3810=PROPERTY_DEFINITION('material property','density of part',#6586);
#3811=PROPERTY_DEFINITION('material property','material name',#6587);
#3812=PROPERTY_DEFINITION('material property','density of part',#6587);
#3813=PROPERTY_DEFINITION('material property','material name',#6588);
#3814=PROPERTY_DEFINITION('material property','density of part',#6588);
#3815=PROPERTY_DEFINITION('material property','material name',#6590);
#3816=PROPERTY_DEFINITION('material property','density of part',#6590);
#3817=PROPERTY_DEFINITION('material property','material name',#6591);
#3818=PROPERTY_DEFINITION('material property','density of part',#6591);
#3819=PROPERTY_DEFINITION('material property','material name',#6593);
#3820=PROPERTY_DEFINITION('material property','density of part',#6593);
#3821=PROPERTY_DEFINITION('material property','material name',#6594);
#3822=PROPERTY_DEFINITION('material property','density of part',#6594);
#3823=PROPERTY_DEFINITION('material property','material name',#6595);
#3824=PROPERTY_DEFINITION('material property','density of part',#6595);
#3825=PROPERTY_DEFINITION('material property','material name',#6596);
#3826=PROPERTY_DEFINITION('material property','density of part',#6596);
#3827=PROPERTY_DEFINITION('material property','material name',#6597);
#3828=PROPERTY_DEFINITION('material property','density of part',#6597);
#3829=PROPERTY_DEFINITION('material property','material name',#6598);
#3830=PROPERTY_DEFINITION('material property','density of part',#6598);
#3831=PROPERTY_DEFINITION('material property','material name',#6599);
#3832=PROPERTY_DEFINITION('material property','density of part',#6599);
#3833=PROPERTY_DEFINITION('material property','material name',#6600);
#3834=PROPERTY_DEFINITION('material property','density of part',#6600);
#3835=AXIS2_PLACEMENT_3D('',#5417,#4267,#4268);
#3836=AXIS2_PLACEMENT_3D('',#5418,#4269,#4270);
#3837=AXIS2_PLACEMENT_3D('',#5419,#4271,#4272);
#3838=AXIS2_PLACEMENT_3D('',#5420,#4273,#4274);
#3839=AXIS2_PLACEMENT_3D('',#5422,#4275,#4276);
#3840=AXIS2_PLACEMENT_3D('',#5425,#4278,#4279);
#3841=AXIS2_PLACEMENT_3D('',#5426,#4280,#4281);
#3842=AXIS2_PLACEMENT_3D('',#5428,#4282,#4283);
#3843=AXIS2_PLACEMENT_3D('',#5431,#4285,#4286);
#3844=AXIS2_PLACEMENT_3D('',#5432,#4287,#4288);
#3845=AXIS2_PLACEMENT_3D('',#5434,#4289,#4290);
#3846=AXIS2_PLACEMENT_3D('',#5437,#4292,#4293);
#3847=AXIS2_PLACEMENT_3D('',#5438,#4294,#4295);
#3848=AXIS2_PLACEMENT_3D('',#5440,#4296,#4297);
#3849=AXIS2_PLACEMENT_3D('',#5443,#4299,#4300);
#3850=AXIS2_PLACEMENT_3D('',#5444,#4301,#4302);
#3851=AXIS2_PLACEMENT_3D('',#5446,#4303,#4304);
#3852=AXIS2_PLACEMENT_3D('',#5449,#4306,#4307);
#3853=AXIS2_PLACEMENT_3D('',#5450,#4308,#4309);
#3854=AXIS2_PLACEMENT_3D('',#5452,#4310,#4311);
#3855=AXIS2_PLACEMENT_3D('',#5455,#4313,#4314);
#3856=AXIS2_PLACEMENT_3D('',#5456,#4315,#4316);
#3857=AXIS2_PLACEMENT_3D('',#5458,#4317,#4318);
#3858=AXIS2_PLACEMENT_3D('',#5461,#4320,#4321);
#3859=AXIS2_PLACEMENT_3D('',#5462,#4322,#4323);
#3860=AXIS2_PLACEMENT_3D('',#5464,#4324,#4325);
#3861=AXIS2_PLACEMENT_3D('',#5467,#4327,#4328);
#3862=AXIS2_PLACEMENT_3D('',#5468,#4329,#4330);
#3863=AXIS2_PLACEMENT_3D('',#5470,#4331,#4332);
#3864=AXIS2_PLACEMENT_3D('',#5473,#4334,#4335);
#3865=AXIS2_PLACEMENT_3D('',#5474,#4336,#4337);
#3866=AXIS2_PLACEMENT_3D('',#5476,#4338,#4339);
#3867=AXIS2_PLACEMENT_3D('',#5479,#4341,#4342);
#3868=AXIS2_PLACEMENT_3D('',#5480,#4343,#4344);
#3869=AXIS2_PLACEMENT_3D('',#5482,#4345,#4346);
#3870=AXIS2_PLACEMENT_3D('',#5485,#4348,#4349);
#3871=AXIS2_PLACEMENT_3D('',#5486,#4350,#4351);
#3872=AXIS2_PLACEMENT_3D('',#5488,#4352,#4353);
#3873=AXIS2_PLACEMENT_3D('',#5491,#4355,#4356);
#3874=AXIS2_PLACEMENT_3D('',#5492,#4357,#4358);
#3875=AXIS2_PLACEMENT_3D('',#5501,#4363,#4364);
#3876=AXIS2_PLACEMENT_3D('',#5507,#4368,#4369);
#3877=AXIS2_PLACEMENT_3D('',#5513,#4373,#4374);
#3878=AXIS2_PLACEMENT_3D('',#5516,#4377,#4378);
#3879=AXIS2_PLACEMENT_3D('',#5517,#4379,#4380);
#3880=AXIS2_PLACEMENT_3D('',#5518,#4381,#4382);
#3881=AXIS2_PLACEMENT_3D('',#5519,#4383,#4384);
#3882=AXIS2_PLACEMENT_3D('',#5521,#4385,#4386);
#3883=AXIS2_PLACEMENT_3D('',#5524,#4388,#4389);
#3884=AXIS2_PLACEMENT_3D('',#5525,#4390,#4391);
#3885=AXIS2_PLACEMENT_3D('',#5527,#4392,#4393);
#3886=AXIS2_PLACEMENT_3D('',#5529,#4395,#4396);
#3887=AXIS2_PLACEMENT_3D('',#5530,#4397,#4398);
#3888=AXIS2_PLACEMENT_3D('',#5532,#4399,#4400);
#3889=AXIS2_PLACEMENT_3D('',#5534,#4402,#4403);
#3890=AXIS2_PLACEMENT_3D('',#5535,#4404,#4405);
#3891=AXIS2_PLACEMENT_3D('',#5536,#4406,#4407);
#3892=AXIS2_PLACEMENT_3D('',#5540,#4409,#4410);
#3893=AXIS2_PLACEMENT_3D('',#5541,#4411,#4412);
#3894=AXIS2_PLACEMENT_3D('',#5545,#4414,#4415);
#3895=AXIS2_PLACEMENT_3D('',#5547,#4417,#4418);
#3896=AXIS2_PLACEMENT_3D('',#5552,#4420,#4421);
#3897=AXIS2_PLACEMENT_3D('',#5555,#4423,#4424);
#3898=AXIS2_PLACEMENT_3D('',#5556,#4425,#4426);
#3899=AXIS2_PLACEMENT_3D('',#5558,#4428,#4429);
#3900=AXIS2_PLACEMENT_3D('',#5569,#4435,#4436);
#3901=AXIS2_PLACEMENT_3D('',#5570,#4437,#4438);
#3902=AXIS2_PLACEMENT_3D('',#5577,#4442,#4443);
#3903=AXIS2_PLACEMENT_3D('',#5578,#4444,#4445);
#3904=AXIS2_PLACEMENT_3D('',#5589,#4451,#4452);
#3905=AXIS2_PLACEMENT_3D('',#5590,#4453,#4454);
#3906=AXIS2_PLACEMENT_3D('',#5592,#4455,#4456);
#3907=AXIS2_PLACEMENT_3D('',#5595,#4458,#4459);
#3908=AXIS2_PLACEMENT_3D('',#5596,#4460,#4461);
#3909=AXIS2_PLACEMENT_3D('',#5599,#4463,#4464);
#3910=AXIS2_PLACEMENT_3D('',#5600,#4465,#4466);
#3911=AXIS2_PLACEMENT_3D('',#5602,#4467,#4468);
#3912=AXIS2_PLACEMENT_3D('',#5604,#4470,#4471);
#3913=AXIS2_PLACEMENT_3D('',#5606,#4472,#4473);
#3914=AXIS2_PLACEMENT_3D('',#5608,#4475,#4476);
#3915=AXIS2_PLACEMENT_3D('',#5610,#4477,#4478);
#3916=AXIS2_PLACEMENT_3D('',#5613,#4480,#4481);
#3917=AXIS2_PLACEMENT_3D('',#5614,#4482,#4483);
#3918=AXIS2_PLACEMENT_3D('',#5631,#4493,#4494);
#3919=AXIS2_PLACEMENT_3D('',#5635,#4497,#4498);
#3920=AXIS2_PLACEMENT_3D('',#5639,#4501,#4502);
#3921=AXIS2_PLACEMENT_3D('',#5641,#4504,#4505);
#3922=AXIS2_PLACEMENT_3D('',#5645,#4508,#4509);
#3923=AXIS2_PLACEMENT_3D('',#5649,#4512,#4513);
#3924=AXIS2_PLACEMENT_3D('',#5653,#4516,#4517);
#3925=AXIS2_PLACEMENT_3D('',#5657,#4520,#4521);
#3926=AXIS2_PLACEMENT_3D('',#5661,#4524,#4525);
#3927=AXIS2_PLACEMENT_3D('',#5663,#4527,#4528);
#3928=AXIS2_PLACEMENT_3D('',#5664,#4529,#4530);
#3929=AXIS2_PLACEMENT_3D('',#5665,#4531,#4532);
#3930=AXIS2_PLACEMENT_3D('',#5674,#4537,#4538);
#3931=AXIS2_PLACEMENT_3D('',#5680,#4542,#4543);
#3932=AXIS2_PLACEMENT_3D('',#5686,#4547,#4548);
#3933=AXIS2_PLACEMENT_3D('',#5692,#4552,#4553);
#3934=AXIS2_PLACEMENT_3D('',#5698,#4557,#4558);
#3935=AXIS2_PLACEMENT_3D('',#5701,#4561,#4562);
#3936=AXIS2_PLACEMENT_3D('',#5702,#4563,#4564);
#3937=AXIS2_PLACEMENT_3D('',#5703,#4565,#4566);
#3938=AXIS2_PLACEMENT_3D('',#5705,#4567,#4568);
#3939=AXIS2_PLACEMENT_3D('',#5706,#4569,#4570);
#3940=AXIS2_PLACEMENT_3D('',#5708,#4571,#4572);
#3941=AXIS2_PLACEMENT_3D('',#5709,#4573,#4574);
#3942=AXIS2_PLACEMENT_3D('',#5711,#4575,#4576);
#3943=AXIS2_PLACEMENT_3D('',#5713,#4578,#4579);
#3944=AXIS2_PLACEMENT_3D('',#5715,#4580,#4581);
#3945=AXIS2_PLACEMENT_3D('',#5717,#4583,#4584);
#3946=AXIS2_PLACEMENT_3D('',#5719,#4585,#4586);
#3947=AXIS2_PLACEMENT_3D('',#5721,#4588,#4589);
#3948=AXIS2_PLACEMENT_3D('',#5723,#4590,#4591);
#3949=AXIS2_PLACEMENT_3D('',#5724,#4592,#4593);
#3950=AXIS2_PLACEMENT_3D('',#5726,#4594,#4595);
#3951=AXIS2_PLACEMENT_3D('',#5728,#4597,#4598);
#3952=AXIS2_PLACEMENT_3D('',#5730,#4600,#4601);
#3953=AXIS2_PLACEMENT_3D('',#5731,#4602,#4603);
#3954=AXIS2_PLACEMENT_3D('',#5733,#4604,#4605);
#3955=AXIS2_PLACEMENT_3D('',#5736,#4607,#4608);
#3956=AXIS2_PLACEMENT_3D('',#5737,#4609,#4610);
#3957=AXIS2_PLACEMENT_3D('',#5739,#4611,#4612);
#3958=AXIS2_PLACEMENT_3D('',#5740,#4613,#4614);
#3959=AXIS2_PLACEMENT_3D('',#5742,#4615,#4616);
#3960=AXIS2_PLACEMENT_3D('',#5745,#4618,#4619);
#3961=AXIS2_PLACEMENT_3D('',#5746,#4620,#4621);
#3962=AXIS2_PLACEMENT_3D('',#5748,#4622,#4623);
#3963=AXIS2_PLACEMENT_3D('',#5749,#4624,#4625);
#3964=AXIS2_PLACEMENT_3D('',#5751,#4626,#4627);
#3965=AXIS2_PLACEMENT_3D('',#5753,#4629,#4630);
#3966=AXIS2_PLACEMENT_3D('',#5755,#4631,#4632);
#3967=AXIS2_PLACEMENT_3D('',#5757,#4634,#4635);
#3968=AXIS2_PLACEMENT_3D('',#5766,#4640,#4641);
#3969=AXIS2_PLACEMENT_3D('',#5772,#4645,#4646);
#3970=AXIS2_PLACEMENT_3D('',#5778,#4650,#4651);
#3971=AXIS2_PLACEMENT_3D('',#5781,#4654,#4655);
#3972=AXIS2_PLACEMENT_3D('',#5782,#4656,#4657);
#3973=AXIS2_PLACEMENT_3D('',#5783,#4658,#4659);
#3974=AXIS2_PLACEMENT_3D('',#5784,#4660,#4661);
#3975=AXIS2_PLACEMENT_3D('',#5793,#4666,#4667);
#3976=AXIS2_PLACEMENT_3D('',#5799,#4671,#4672);
#3977=AXIS2_PLACEMENT_3D('',#5805,#4676,#4677);
#3978=AXIS2_PLACEMENT_3D('',#5808,#4680,#4681);
#3979=AXIS2_PLACEMENT_3D('',#5809,#4682,#4683);
#3980=AXIS2_PLACEMENT_3D('',#5810,#4684,#4685);
#3981=AXIS2_PLACEMENT_3D('',#5811,#4686,#4687);
#3982=AXIS2_PLACEMENT_3D('',#5812,#4688,#4689);
#3983=AXIS2_PLACEMENT_3D('',#5814,#4690,#4691);
#3984=AXIS2_PLACEMENT_3D('',#5817,#4693,#4694);
#3985=AXIS2_PLACEMENT_3D('',#5818,#4695,#4696);
#3986=AXIS2_PLACEMENT_3D('',#5820,#4697,#4698);
#3987=AXIS2_PLACEMENT_3D('',#5823,#4700,#4701);
#3988=AXIS2_PLACEMENT_3D('',#5824,#4702,#4703);
#3989=AXIS2_PLACEMENT_3D('',#5826,#4704,#4705);
#3990=AXIS2_PLACEMENT_3D('',#5829,#4707,#4708);
#3991=AXIS2_PLACEMENT_3D('',#5830,#4709,#4710);
#3992=AXIS2_PLACEMENT_3D('',#5832,#4711,#4712);
#3993=AXIS2_PLACEMENT_3D('',#5835,#4714,#4715);
#3994=AXIS2_PLACEMENT_3D('',#5836,#4716,#4717);
#3995=AXIS2_PLACEMENT_3D('',#5838,#4718,#4719);
#3996=AXIS2_PLACEMENT_3D('',#5841,#4721,#4722);
#3997=AXIS2_PLACEMENT_3D('',#5842,#4723,#4724);
#3998=AXIS2_PLACEMENT_3D('',#5843,#4725,#4726);
#3999=AXIS2_PLACEMENT_3D('',#5845,#4727,#4728);
#4000=AXIS2_PLACEMENT_3D('',#5848,#4730,#4731);
#4001=AXIS2_PLACEMENT_3D('',#5849,#4732,#4733);
#4002=AXIS2_PLACEMENT_3D('',#5850,#4734,#4735);
#4003=AXIS2_PLACEMENT_3D('',#5852,#4736,#4737);
#4004=AXIS2_PLACEMENT_3D('',#5855,#4739,#4740);
#4005=AXIS2_PLACEMENT_3D('',#5856,#4741,#4742);
#4006=AXIS2_PLACEMENT_3D('',#5857,#4743,#4744);
#4007=AXIS2_PLACEMENT_3D('',#5859,#4745,#4746);
#4008=AXIS2_PLACEMENT_3D('',#5862,#4748,#4749);
#4009=AXIS2_PLACEMENT_3D('',#5863,#4750,#4751);
#4010=AXIS2_PLACEMENT_3D('',#5864,#4752,#4753);
#4011=AXIS2_PLACEMENT_3D('',#5866,#4754,#4755);
#4012=AXIS2_PLACEMENT_3D('',#5869,#4757,#4758);
#4013=AXIS2_PLACEMENT_3D('',#5870,#4759,#4760);
#4014=AXIS2_PLACEMENT_3D('',#5872,#4761,#4762);
#4015=AXIS2_PLACEMENT_3D('',#5875,#4764,#4765);
#4016=AXIS2_PLACEMENT_3D('',#5876,#4766,#4767);
#4017=AXIS2_PLACEMENT_3D('',#5885,#4772,#4773);
#4018=AXIS2_PLACEMENT_3D('',#5891,#4777,#4778);
#4019=AXIS2_PLACEMENT_3D('',#5897,#4782,#4783);
#4020=AXIS2_PLACEMENT_3D('',#5900,#4786,#4787);
#4021=AXIS2_PLACEMENT_3D('',#5901,#4788,#4789);
#4022=AXIS2_PLACEMENT_3D('',#5902,#4790,#4791);
#4023=AXIS2_PLACEMENT_3D('',#5903,#4792,#4793);
#4024=AXIS2_PLACEMENT_3D('',#5905,#4794,#4795);
#4025=AXIS2_PLACEMENT_3D('',#5908,#4797,#4798);
#4026=AXIS2_PLACEMENT_3D('',#5909,#4799,#4800);
#4027=AXIS2_PLACEMENT_3D('',#5911,#4801,#4802);
#4028=AXIS2_PLACEMENT_3D('',#5914,#4804,#4805);
#4029=AXIS2_PLACEMENT_3D('',#5915,#4806,#4807);
#4030=AXIS2_PLACEMENT_3D('',#5917,#4808,#4809);
#4031=AXIS2_PLACEMENT_3D('',#5920,#4811,#4812);
#4032=AXIS2_PLACEMENT_3D('',#5921,#4813,#4814);
#4033=AXIS2_PLACEMENT_3D('',#5923,#4815,#4816);
#4034=AXIS2_PLACEMENT_3D('',#5926,#4818,#4819);
#4035=AXIS2_PLACEMENT_3D('',#5927,#4820,#4821);
#4036=AXIS2_PLACEMENT_3D('',#5929,#4822,#4823);
#4037=AXIS2_PLACEMENT_3D('',#5932,#4825,#4826);
#4038=AXIS2_PLACEMENT_3D('',#5933,#4827,#4828);
#4039=AXIS2_PLACEMENT_3D('',#5942,#4833,#4834);
#4040=AXIS2_PLACEMENT_3D('',#5948,#4838,#4839);
#4041=AXIS2_PLACEMENT_3D('',#5954,#4843,#4844);
#4042=AXIS2_PLACEMENT_3D('',#5957,#4847,#4848);
#4043=AXIS2_PLACEMENT_3D('',#5958,#4849,#4850);
#4044=AXIS2_PLACEMENT_3D('',#5959,#4851,#4852);
#4045=AXIS2_PLACEMENT_3D('',#5960,#4853,#4854);
#4046=AXIS2_PLACEMENT_3D('',#5961,#4855,#4856);
#4047=AXIS2_PLACEMENT_3D('',#5964,#4857,#4858);
#4048=AXIS2_PLACEMENT_3D('',#5970,#4862,#4863);
#4049=AXIS2_PLACEMENT_3D('',#5976,#4867,#4868);
#4050=AXIS2_PLACEMENT_3D('',#5978,#4869,#4870);
#4051=AXIS2_PLACEMENT_3D('',#5982,#4873,#4874);
#4052=AXIS2_PLACEMENT_3D('',#5985,#4877,#4878);
#4053=AXIS2_PLACEMENT_3D('',#5986,#4879,#4880);
#4054=AXIS2_PLACEMENT_3D('',#5988,#4881,#4882);
#4055=AXIS2_PLACEMENT_3D('',#5990,#4883,#4884);
#4056=AXIS2_PLACEMENT_3D('',#5991,#4885,#4886);
#4057=AXIS2_PLACEMENT_3D('',#5993,#4887,#4888);
#4058=AXIS2_PLACEMENT_3D('',#5995,#4890,#4891);
#4059=AXIS2_PLACEMENT_3D('',#5997,#4892,#4893);
#4060=AXIS2_PLACEMENT_3D('',#5998,#4894,#4895);
#4061=AXIS2_PLACEMENT_3D('',#6000,#4896,#4897);
#4062=AXIS2_PLACEMENT_3D('',#6002,#4899,#4900);
#4063=AXIS2_PLACEMENT_3D('',#6004,#4901,#4902);
#4064=AXIS2_PLACEMENT_3D('',#6005,#4903,#4904);
#4065=AXIS2_PLACEMENT_3D('',#6007,#4905,#4906);
#4066=AXIS2_PLACEMENT_3D('',#6009,#4908,#4909);
#4067=AXIS2_PLACEMENT_3D('',#6011,#4910,#4911);
#4068=AXIS2_PLACEMENT_3D('',#6012,#4912,#4913);
#4069=AXIS2_PLACEMENT_3D('',#6014,#4914,#4915);
#4070=AXIS2_PLACEMENT_3D('',#6016,#4917,#4918);
#4071=AXIS2_PLACEMENT_3D('',#6018,#4919,#4920);
#4072=AXIS2_PLACEMENT_3D('',#6019,#4921,#4922);
#4073=AXIS2_PLACEMENT_3D('',#6021,#4923,#4924);
#4074=AXIS2_PLACEMENT_3D('',#6023,#4926,#4927);
#4075=AXIS2_PLACEMENT_3D('',#6025,#4928,#4929);
#4076=AXIS2_PLACEMENT_3D('',#6026,#4930,#4931);
#4077=AXIS2_PLACEMENT_3D('',#6028,#4933,#4934);
#4078=AXIS2_PLACEMENT_3D('',#6029,#4935,#4936);
#4079=AXIS2_PLACEMENT_3D('',#6032,#4937,#4938);
#4080=AXIS2_PLACEMENT_3D('',#6036,#4940,#4941);
#4081=AXIS2_PLACEMENT_3D('',#6038,#4943,#4944);
#4082=AXIS2_PLACEMENT_3D('',#6044,#4948,#4949);
#4083=AXIS2_PLACEMENT_3D('',#6046,#4950,#4951);
#4084=AXIS2_PLACEMENT_3D('',#6048,#4952,#4953);
#4085=AXIS2_PLACEMENT_3D('',#6050,#4955,#4956);
#4086=AXIS2_PLACEMENT_3D('',#6053,#4959,#4960);
#4087=AXIS2_PLACEMENT_3D('',#6055,#4961,#4962);
#4088=AXIS2_PLACEMENT_3D('',#6057,#4963,#4964);
#4089=AXIS2_PLACEMENT_3D('',#6058,#4965,#4966);
#4090=AXIS2_PLACEMENT_3D('',#6060,#4967,#4968);
#4091=AXIS2_PLACEMENT_3D('',#6062,#4970,#4971);
#4092=AXIS2_PLACEMENT_3D('',#6064,#4972,#4973);
#4093=AXIS2_PLACEMENT_3D('',#6065,#4974,#4975);
#4094=AXIS2_PLACEMENT_3D('',#6067,#4977,#4978);
#4095=AXIS2_PLACEMENT_3D('',#6068,#4979,#4980);
#4096=AXIS2_PLACEMENT_3D('',#6069,#4981,#4982);
#4097=AXIS2_PLACEMENT_3D('',#6070,#4983,#4984);
#4098=AXIS2_PLACEMENT_3D('',#6072,#4985,#4986);
#4099=AXIS2_PLACEMENT_3D('',#6075,#4988,#4989);
#4100=AXIS2_PLACEMENT_3D('',#6076,#4990,#4991);
#4101=AXIS2_PLACEMENT_3D('',#6078,#4992,#4993);
#4102=AXIS2_PLACEMENT_3D('',#6081,#4995,#4996);
#4103=AXIS2_PLACEMENT_3D('',#6082,#4997,#4998);
#4104=AXIS2_PLACEMENT_3D('',#6084,#4999,#5000);
#4105=AXIS2_PLACEMENT_3D('',#6087,#5002,#5003);
#4106=AXIS2_PLACEMENT_3D('',#6088,#5004,#5005);
#4107=AXIS2_PLACEMENT_3D('',#6090,#5006,#5007);
#4108=AXIS2_PLACEMENT_3D('',#6093,#5009,#5010);
#4109=AXIS2_PLACEMENT_3D('',#6094,#5011,#5012);
#4110=AXIS2_PLACEMENT_3D('',#6096,#5013,#5014);
#4111=AXIS2_PLACEMENT_3D('',#6099,#5016,#5017);
#4112=AXIS2_PLACEMENT_3D('',#6100,#5018,#5019);
#4113=AXIS2_PLACEMENT_3D('',#6102,#5020,#5021);
#4114=AXIS2_PLACEMENT_3D('',#6105,#5023,#5024);
#4115=AXIS2_PLACEMENT_3D('',#6106,#5025,#5026);
#4116=AXIS2_PLACEMENT_3D('',#6115,#5031,#5032);
#4117=AXIS2_PLACEMENT_3D('',#6121,#5036,#5037);
#4118=AXIS2_PLACEMENT_3D('',#6127,#5041,#5042);
#4119=AXIS2_PLACEMENT_3D('',#6130,#5045,#5046);
#4120=AXIS2_PLACEMENT_3D('',#6131,#5047,#5048);
#4121=AXIS2_PLACEMENT_3D('',#6132,#5049,#5050);
#4122=AXIS2_PLACEMENT_3D('',#6133,#5051,#5052);
#4123=AXIS2_PLACEMENT_3D('',#6135,#5053,#5054);
#4124=AXIS2_PLACEMENT_3D('',#6136,#5055,#5056);
#4125=AXIS2_PLACEMENT_3D('',#6138,#5057,#5058);
#4126=AXIS2_PLACEMENT_3D('',#6140,#5060,#5061);
#4127=AXIS2_PLACEMENT_3D('',#6142,#5062,#5063);
#4128=AXIS2_PLACEMENT_3D('',#6144,#5065,#5066);
#4129=AXIS2_PLACEMENT_3D('',#6146,#5067,#5068);
#4130=AXIS2_PLACEMENT_3D('',#6148,#5070,#5071);
#4131=AXIS2_PLACEMENT_3D('',#6150,#5072,#5073);
#4132=AXIS2_PLACEMENT_3D('',#6151,#5074,#5075);
#4133=AXIS2_PLACEMENT_3D('',#6153,#5076,#5077);
#4134=AXIS2_PLACEMENT_3D('',#6155,#5079,#5080);
#4135=AXIS2_PLACEMENT_3D('',#6157,#5081,#5082);
#4136=AXIS2_PLACEMENT_3D('',#6159,#5084,#5085);
#4137=AXIS2_PLACEMENT_3D('',#6161,#5086,#5087);
#4138=AXIS2_PLACEMENT_3D('',#6163,#5089,#5090);
#4139=AXIS2_PLACEMENT_3D('',#6164,#5091,#5092);
#4140=AXIS2_PLACEMENT_3D('',#6173,#5097,#5098);
#4141=AXIS2_PLACEMENT_3D('',#6179,#5102,#5103);
#4142=AXIS2_PLACEMENT_3D('',#6185,#5107,#5108);
#4143=AXIS2_PLACEMENT_3D('',#6191,#5112,#5113);
#4144=AXIS2_PLACEMENT_3D('',#6197,#5117,#5118);
#4145=AXIS2_PLACEMENT_3D('',#6200,#5121,#5122);
#4146=AXIS2_PLACEMENT_3D('',#6201,#5123,#5124);
#4147=AXIS2_PLACEMENT_3D('',#6202,#5125,#5126);
#4148=AXIS2_PLACEMENT_3D('',#6203,#5127,#5128);
#4149=AXIS2_PLACEMENT_3D('',#6205,#5129,#5130);
#4150=AXIS2_PLACEMENT_3D('',#6206,#5131,#5132);
#4151=AXIS2_PLACEMENT_3D('',#6208,#5133,#5134);
#4152=AXIS2_PLACEMENT_3D('',#6210,#5136,#5137);
#4153=AXIS2_PLACEMENT_3D('',#6212,#5138,#5139);
#4154=AXIS2_PLACEMENT_3D('',#6214,#5141,#5142);
#4155=AXIS2_PLACEMENT_3D('',#6216,#5143,#5144);
#4156=AXIS2_PLACEMENT_3D('',#6218,#5146,#5147);
#4157=AXIS2_PLACEMENT_3D('',#6220,#5148,#5149);
#4158=AXIS2_PLACEMENT_3D('',#6221,#5150,#5151);
#4159=AXIS2_PLACEMENT_3D('',#6223,#5152,#5153);
#4160=AXIS2_PLACEMENT_3D('',#6225,#5155,#5156);
#4161=AXIS2_PLACEMENT_3D('',#6227,#5157,#5158);
#4162=AXIS2_PLACEMENT_3D('',#6229,#5160,#5161);
#4163=AXIS2_PLACEMENT_3D('',#6231,#5162,#5163);
#4164=AXIS2_PLACEMENT_3D('',#6233,#5165,#5166);
#4165=AXIS2_PLACEMENT_3D('',#6234,#5167,#5168);
#4166=AXIS2_PLACEMENT_3D('',#6243,#5173,#5174);
#4167=AXIS2_PLACEMENT_3D('',#6249,#5178,#5179);
#4168=AXIS2_PLACEMENT_3D('',#6255,#5183,#5184);
#4169=AXIS2_PLACEMENT_3D('',#6261,#5188,#5189);
#4170=AXIS2_PLACEMENT_3D('',#6267,#5193,#5194);
#4171=AXIS2_PLACEMENT_3D('',#6270,#5197,#5198);
#4172=AXIS2_PLACEMENT_3D('',#6271,#5199,#5200);
#4173=AXIS2_PLACEMENT_3D('',#6272,#5201,#5202);
#4174=AXIS2_PLACEMENT_3D('',#6273,#5203,#5204);
#4175=AXIS2_PLACEMENT_3D('',#6274,#5205,#5206);
#4176=AXIS2_PLACEMENT_3D('',#6275,#5207,#5208);
#4177=AXIS2_PLACEMENT_3D('',#6276,#5209,#5210);
#4178=AXIS2_PLACEMENT_3D('',#6277,#5211,#5212);
#4179=AXIS2_PLACEMENT_3D('',#6278,#5213,#5214);
#4180=AXIS2_PLACEMENT_3D('',#6279,#5215,#5216);
#4181=AXIS2_PLACEMENT_3D('',#6280,#5217,#5218);
#4182=AXIS2_PLACEMENT_3D('',#6281,#5219,#5220);
#4183=AXIS2_PLACEMENT_3D('',#6282,#5221,#5222);
#4184=AXIS2_PLACEMENT_3D('',#6283,#5223,#5224);
#4185=AXIS2_PLACEMENT_3D('',#6284,#5225,#5226);
#4186=AXIS2_PLACEMENT_3D('',#6285,#5227,#5228);
#4187=AXIS2_PLACEMENT_3D('',#6286,#5229,#5230);
#4188=AXIS2_PLACEMENT_3D('',#6287,#5231,#5232);
#4189=AXIS2_PLACEMENT_3D('',#6288,#5233,#5234);
#4190=AXIS2_PLACEMENT_3D('',#6289,#5235,#5236);
#4191=AXIS2_PLACEMENT_3D('',#6290,#5237,#5238);
#4192=AXIS2_PLACEMENT_3D('',#6291,#5239,#5240);
#4193=AXIS2_PLACEMENT_3D('',#6292,#5241,#5242);
#4194=AXIS2_PLACEMENT_3D('',#6293,#5243,#5244);
#4195=AXIS2_PLACEMENT_3D('',#6294,#5245,#5246);
#4196=AXIS2_PLACEMENT_3D('',#6295,#5247,#5248);
#4197=AXIS2_PLACEMENT_3D('',#6296,#5249,#5250);
#4198=AXIS2_PLACEMENT_3D('',#6297,#5251,#5252);
#4199=AXIS2_PLACEMENT_3D('',#6298,#5253,#5254);
#4200=AXIS2_PLACEMENT_3D('',#6299,#5255,#5256);
#4201=AXIS2_PLACEMENT_3D('',#6300,#5257,#5258);
#4202=AXIS2_PLACEMENT_3D('',#6302,#5259,#5260);
#4203=AXIS2_PLACEMENT_3D('',#6305,#5262,#5263);
#4204=AXIS2_PLACEMENT_3D('',#6306,#5264,#5265);
#4205=AXIS2_PLACEMENT_3D('',#6308,#5266,#5267);
#4206=AXIS2_PLACEMENT_3D('',#6311,#5269,#5270);
#4207=AXIS2_PLACEMENT_3D('',#6312,#5271,#5272);
#4208=AXIS2_PLACEMENT_3D('',#6313,#5273,#5274);
#4209=AXIS2_PLACEMENT_3D('',#6314,#5275,#5276);
#4210=AXIS2_PLACEMENT_3D('',#6315,#5277,#5278);
#4211=AXIS2_PLACEMENT_3D('',#6317,#5279,#5280);
#4212=AXIS2_PLACEMENT_3D('',#6320,#5282,#5283);
#4213=AXIS2_PLACEMENT_3D('',#6321,#5284,#5285);
#4214=AXIS2_PLACEMENT_3D('',#6323,#5286,#5287);
#4215=AXIS2_PLACEMENT_3D('',#6326,#5289,#5290);
#4216=AXIS2_PLACEMENT_3D('',#6327,#5291,#5292);
#4217=AXIS2_PLACEMENT_3D('',#6328,#5293,#5294);
#4218=AXIS2_PLACEMENT_3D('',#6329,#5295,#5296);
#4219=AXIS2_PLACEMENT_3D('',#6330,#5297,#5298);
#4220=AXIS2_PLACEMENT_3D('',#6332,#5299,#5300);
#4221=AXIS2_PLACEMENT_3D('',#6333,#5301,#5302);
#4222=AXIS2_PLACEMENT_3D('',#6335,#5303,#5304);
#4223=AXIS2_PLACEMENT_3D('',#6337,#5306,#5307);
#4224=AXIS2_PLACEMENT_3D('',#6339,#5308,#5309);
#4225=AXIS2_PLACEMENT_3D('',#6341,#5311,#5312);
#4226=AXIS2_PLACEMENT_3D('',#6343,#5313,#5314);
#4227=AXIS2_PLACEMENT_3D('',#6345,#5316,#5317);
#4228=AXIS2_PLACEMENT_3D('',#6347,#5318,#5319);
#4229=AXIS2_PLACEMENT_3D('',#6348,#5320,#5321);
#4230=AXIS2_PLACEMENT_3D('',#6350,#5322,#5323);
#4231=AXIS2_PLACEMENT_3D('',#6352,#5325,#5326);
#4232=AXIS2_PLACEMENT_3D('',#6354,#5327,#5328);
#4233=AXIS2_PLACEMENT_3D('',#6356,#5330,#5331);
#4234=AXIS2_PLACEMENT_3D('',#6358,#5332,#5333);
#4235=AXIS2_PLACEMENT_3D('',#6360,#5335,#5336);
#4236=AXIS2_PLACEMENT_3D('',#6361,#5337,#5338);
#4237=AXIS2_PLACEMENT_3D('',#6370,#5343,#5344);
#4238=AXIS2_PLACEMENT_3D('',#6376,#5348,#5349);
#4239=AXIS2_PLACEMENT_3D('',#6382,#5353,#5354);
#4240=AXIS2_PLACEMENT_3D('',#6388,#5358,#5359);
#4241=AXIS2_PLACEMENT_3D('',#6394,#5363,#5364);
#4242=AXIS2_PLACEMENT_3D('',#6397,#5367,#5368);
#4243=AXIS2_PLACEMENT_3D('',#6398,#5369,#5370);
#4244=AXIS2_PLACEMENT_3D('',#6399,#5371,#5372);
#4245=AXIS2_PLACEMENT_3D('',#6400,#5373,#5374);
#4246=AXIS2_PLACEMENT_3D('',#6401,#5375,#5376);
#4247=AXIS2_PLACEMENT_3D('',#6402,#5377,#5378);
#4248=AXIS2_PLACEMENT_3D('',#6403,#5379,#5380);
#4249=AXIS2_PLACEMENT_3D('',#6404,#5381,#5382);
#4250=AXIS2_PLACEMENT_3D('',#6405,#5383,#5384);
#4251=AXIS2_PLACEMENT_3D('',#6406,#5385,#5386);
#4252=AXIS2_PLACEMENT_3D('',#6407,#5387,#5388);
#4253=AXIS2_PLACEMENT_3D('',#6408,#5389,#5390);
#4254=AXIS2_PLACEMENT_3D('',#6409,#5391,#5392);
#4255=AXIS2_PLACEMENT_3D('',#6410,#5393,#5394);
#4256=AXIS2_PLACEMENT_3D('',#6411,#5395,#5396);
#4257=AXIS2_PLACEMENT_3D('',#6412,#5397,#5398);
#4258=AXIS2_PLACEMENT_3D('',#6413,#5399,#5400);
#4259=AXIS2_PLACEMENT_3D('',#6414,#5401,#5402);
#4260=AXIS2_PLACEMENT_3D('',#6415,#5403,#5404);
#4261=AXIS2_PLACEMENT_3D('',#6416,#5405,#5406);
#4262=AXIS2_PLACEMENT_3D('',#6417,#5407,#5408);
#4263=AXIS2_PLACEMENT_3D('',#6418,#5409,#5410);
#4264=AXIS2_PLACEMENT_3D('',#6419,#5411,#5412);
#4265=AXIS2_PLACEMENT_3D('',#6420,#5413,#5414);
#4266=AXIS2_PLACEMENT_3D('',#6421,#5415,#5416);
#4267=DIRECTION('axis',(0.,0.,1.));
#4268=DIRECTION('refdir',(1.,0.,0.));
#4269=DIRECTION('axis',(0.,0.,1.));
#4270=DIRECTION('refdir',(1.,0.,0.));
#4271=DIRECTION('axis',(0.,0.,1.));
#4272=DIRECTION('refdir',(1.,0.,0.));
#4273=DIRECTION('center_axis',(0.,0.,1.));
#4274=DIRECTION('ref_axis',(1.,0.,0.));
#4275=DIRECTION('center_axis',(0.,0.,1.));
#4276=DIRECTION('ref_axis',(1.,0.,0.));
#4277=DIRECTION('',(0.,0.,1.));
#4278=DIRECTION('center_axis',(0.,0.,-1.));
#4279=DIRECTION('ref_axis',(1.,0.,0.));
#4280=DIRECTION('center_axis',(0.,0.,1.));
#4281=DIRECTION('ref_axis',(1.,0.,0.));
#4282=DIRECTION('center_axis',(0.,0.,1.));
#4283=DIRECTION('ref_axis',(1.,0.,0.));
#4284=DIRECTION('',(0.,0.,1.));
#4285=DIRECTION('center_axis',(0.,0.,-1.));
#4286=DIRECTION('ref_axis',(1.,0.,0.));
#4287=DIRECTION('center_axis',(0.,0.,1.));
#4288=DIRECTION('ref_axis',(1.,0.,0.));
#4289=DIRECTION('center_axis',(0.,0.,1.));
#4290=DIRECTION('ref_axis',(1.,0.,0.));
#4291=DIRECTION('',(0.,0.,1.));
#4292=DIRECTION('center_axis',(0.,0.,-1.));
#4293=DIRECTION('ref_axis',(1.,0.,0.));
#4294=DIRECTION('center_axis',(0.,0.,1.));
#4295=DIRECTION('ref_axis',(1.,0.,0.));
#4296=DIRECTION('center_axis',(0.,0.,1.));
#4297=DIRECTION('ref_axis',(1.,0.,0.));
#4298=DIRECTION('',(0.,0.,1.));
#4299=DIRECTION('center_axis',(0.,0.,-1.));
#4300=DIRECTION('ref_axis',(1.,0.,0.));
#4301=DIRECTION('center_axis',(0.,0.,1.));
#4302=DIRECTION('ref_axis',(1.,0.,0.));
#4303=DIRECTION('center_axis',(0.,0.,1.));
#4304=DIRECTION('ref_axis',(1.,0.,0.));
#4305=DIRECTION('',(0.,0.,1.));
#4306=DIRECTION('center_axis',(0.,0.,-1.));
#4307=DIRECTION('ref_axis',(1.,0.,0.));
#4308=DIRECTION('center_axis',(0.,0.,1.));
#4309=DIRECTION('ref_axis',(1.,0.,0.));
#4310=DIRECTION('center_axis',(0.,0.,1.));
#4311=DIRECTION('ref_axis',(1.,0.,0.));
#4312=DIRECTION('',(0.,0.,1.));
#4313=DIRECTION('center_axis',(0.,0.,-1.));
#4314=DIRECTION('ref_axis',(1.,0.,0.));
#4315=DIRECTION('center_axis',(0.,0.,1.));
#4316=DIRECTION('ref_axis',(1.,0.,0.));
#4317=DIRECTION('center_axis',(0.,0.,1.));
#4318=DIRECTION('ref_axis',(1.,0.,0.));
#4319=DIRECTION('',(0.,0.,1.));
#4320=DIRECTION('center_axis',(0.,0.,-1.));
#4321=DIRECTION('ref_axis',(1.,0.,0.));
#4322=DIRECTION('center_axis',(0.,0.,1.));
#4323=DIRECTION('ref_axis',(1.,0.,0.));
#4324=DIRECTION('center_axis',(0.,0.,1.));
#4325=DIRECTION('ref_axis',(1.,0.,0.));
#4326=DIRECTION('',(0.,0.,1.));
#4327=DIRECTION('center_axis',(0.,0.,-1.));
#4328=DIRECTION('ref_axis',(1.,0.,0.));
#4329=DIRECTION('center_axis',(0.,0.,1.));
#4330=DIRECTION('ref_axis',(1.,0.,0.));
#4331=DIRECTION('center_axis',(0.,0.,1.));
#4332=DIRECTION('ref_axis',(1.,0.,0.));
#4333=DIRECTION('',(0.,0.,1.));
#4334=DIRECTION('center_axis',(0.,0.,-1.));
#4335=DIRECTION('ref_axis',(1.,0.,0.));
#4336=DIRECTION('center_axis',(0.,0.,1.));
#4337=DIRECTION('ref_axis',(1.,0.,0.));
#4338=DIRECTION('center_axis',(0.,0.,1.));
#4339=DIRECTION('ref_axis',(1.,0.,0.));
#4340=DIRECTION('',(0.,0.,1.));
#4341=DIRECTION('center_axis',(0.,0.,-1.));
#4342=DIRECTION('ref_axis',(1.,0.,0.));
#4343=DIRECTION('center_axis',(0.,0.,1.));
#4344=DIRECTION('ref_axis',(1.,0.,0.));
#4345=DIRECTION('center_axis',(0.,0.,1.));
#4346=DIRECTION('ref_axis',(1.,0.,0.));
#4347=DIRECTION('',(0.,0.,1.));
#4348=DIRECTION('center_axis',(0.,0.,-1.));
#4349=DIRECTION('ref_axis',(1.,0.,0.));
#4350=DIRECTION('center_axis',(0.,0.,1.));
#4351=DIRECTION('ref_axis',(1.,0.,0.));
#4352=DIRECTION('center_axis',(0.,0.,1.));
#4353=DIRECTION('ref_axis',(1.,0.,0.));
#4354=DIRECTION('',(0.,0.,1.));
#4355=DIRECTION('center_axis',(0.,0.,-1.));
#4356=DIRECTION('ref_axis',(1.,0.,0.));
#4357=DIRECTION('center_axis',(0.,1.,0.));
#4358=DIRECTION('ref_axis',(-1.,0.,0.));
#4359=DIRECTION('',(-1.,0.,0.));
#4360=DIRECTION('',(0.,0.,1.));
#4361=DIRECTION('',(-1.,0.,0.));
#4362=DIRECTION('',(0.,0.,1.));
#4363=DIRECTION('center_axis',(1.,0.,0.));
#4364=DIRECTION('ref_axis',(0.,1.,0.));
#4365=DIRECTION('',(0.,1.,0.));
#4366=DIRECTION('',(0.,1.,0.));
#4367=DIRECTION('',(0.,0.,1.));
#4368=DIRECTION('center_axis',(0.,-1.,0.));
#4369=DIRECTION('ref_axis',(1.,0.,0.));
#4370=DIRECTION('',(1.,0.,0.));
#4371=DIRECTION('',(1.,0.,0.));
#4372=DIRECTION('',(0.,0.,1.));
#4373=DIRECTION('center_axis',(-1.,0.,0.));
#4374=DIRECTION('ref_axis',(0.,-1.,0.));
#4375=DIRECTION('',(0.,-1.,0.));
#4376=DIRECTION('',(0.,-1.,0.));
#4377=DIRECTION('center_axis',(0.,0.,1.));
#4378=DIRECTION('ref_axis',(1.,0.,0.));
#4379=DIRECTION('center_axis',(0.,0.,1.));
#4380=DIRECTION('ref_axis',(1.,0.,0.));
#4381=DIRECTION('axis',(0.,0.,1.));
#4382=DIRECTION('refdir',(1.,0.,0.));
#4383=DIRECTION('center_axis',(1.,0.,0.));
#4384=DIRECTION('ref_axis',(0.,0.,-1.));
#4385=DIRECTION('center_axis',(-1.,0.,0.));
#4386=DIRECTION('ref_axis',(0.,0.,-1.));
#4387=DIRECTION('',(-0.707106781186548,8.65956056235493E-17,-0.707106781186547));
#4388=DIRECTION('center_axis',(1.,0.,0.));
#4389=DIRECTION('ref_axis',(0.,0.,-1.));
#4390=DIRECTION('center_axis',(1.,0.,0.));
#4391=DIRECTION('ref_axis',(0.,0.,-1.));
#4392=DIRECTION('center_axis',(1.,0.,0.));
#4393=DIRECTION('ref_axis',(0.,0.,-1.));
#4394=DIRECTION('',(-1.,0.,0.));
#4395=DIRECTION('center_axis',(1.,0.,0.));
#4396=DIRECTION('ref_axis',(0.,0.,-1.));
#4397=DIRECTION('center_axis',(-1.,0.,0.));
#4398=DIRECTION('ref_axis',(0.,0.,-1.));
#4399=DIRECTION('center_axis',(-1.,0.,0.));
#4400=DIRECTION('ref_axis',(0.,0.,-1.));
#4401=DIRECTION('',(-0.707106781186553,-8.65956056235487E-17,0.707106781186542));
#4402=DIRECTION('center_axis',(1.,0.,0.));
#4403=DIRECTION('ref_axis',(0.,0.,-1.));
#4404=DIRECTION('axis',(0.,0.,1.));
#4405=DIRECTION('refdir',(1.,0.,0.));
#4406=DIRECTION('center_axis',(0.,0.,1.));
#4407=DIRECTION('ref_axis',(1.,0.,0.));
#4408=DIRECTION('',(0.,-1.,0.));
#4409=DIRECTION('center_axis',(0.,0.,1.));
#4410=DIRECTION('ref_axis',(1.,0.,0.));
#4411=DIRECTION('center_axis',(0.,0.,1.));
#4412=DIRECTION('ref_axis',(1.,0.,0.));
#4413=DIRECTION('',(0.,0.,1.));
#4414=DIRECTION('center_axis',(0.,0.,1.));
#4415=DIRECTION('ref_axis',(1.,0.,0.));
#4416=DIRECTION('',(0.,0.,-1.));
#4417=DIRECTION('center_axis',(0.,0.,1.));
#4418=DIRECTION('ref_axis',(-1.,1.22464679914735E-16,0.));
#4419=DIRECTION('',(0.,0.,-1.));
#4420=DIRECTION('center_axis',(0.,0.,1.));
#4421=DIRECTION('ref_axis',(1.,0.,0.));
#4422=DIRECTION('',(0.,0.,1.));
#4423=DIRECTION('center_axis',(0.,0.,1.));
#4424=DIRECTION('ref_axis',(1.,0.,0.));
#4425=DIRECTION('center_axis',(0.,0.,1.));
#4426=DIRECTION('ref_axis',(1.,0.,0.));
#4427=DIRECTION('',(0.,1.,0.));
#4428=DIRECTION('center_axis',(0.,0.,1.));
#4429=DIRECTION('ref_axis',(1.,0.,0.));
#4430=DIRECTION('',(0.,1.,0.));
#4431=DIRECTION('',(1.,0.,0.));
#4432=DIRECTION('',(0.,-1.,0.));
#4433=DIRECTION('',(-1.,0.,0.));
#4434=DIRECTION('',(0.,1.,0.));
#4435=DIRECTION('center_axis',(0.,0.,-1.));
#4436=DIRECTION('ref_axis',(1.,0.,0.));
#4437=DIRECTION('center_axis',(-1.,0.,0.));
#4438=DIRECTION('ref_axis',(0.,0.,1.));
#4439=DIRECTION('',(0.,0.,-1.));
#4440=DIRECTION('',(0.,1.,0.));
#4441=DIRECTION('',(0.,0.,1.));
#4442=DIRECTION('center_axis',(1.,0.,0.));
#4443=DIRECTION('ref_axis',(0.,0.,-1.));
#4444=DIRECTION('center_axis',(0.,0.,1.));
#4445=DIRECTION('ref_axis',(1.,0.,0.));
#4446=DIRECTION('',(0.,1.,0.));
#4447=DIRECTION('',(1.,0.,0.));
#4448=DIRECTION('',(0.,1.,0.));
#4449=DIRECTION('',(0.,1.,0.));
#4450=DIRECTION('',(-1.,0.,0.));
#4451=DIRECTION('center_axis',(0.,0.,-1.));
#4452=DIRECTION('ref_axis',(1.,0.,0.));
#4453=DIRECTION('center_axis',(1.,0.,0.));
#4454=DIRECTION('ref_axis',(0.,0.,-1.));
#4455=DIRECTION('center_axis',(1.,0.,0.));
#4456=DIRECTION('ref_axis',(0.,0.,-1.));
#4457=DIRECTION('',(1.,0.,0.));
#4458=DIRECTION('center_axis',(-1.,0.,0.));
#4459=DIRECTION('ref_axis',(0.,0.,-1.));
#4460=DIRECTION('center_axis',(1.,0.,0.));
#4461=DIRECTION('ref_axis',(0.,0.,-1.));
#4462=DIRECTION('',(1.,0.,0.));
#4463=DIRECTION('center_axis',(-1.,0.,0.));
#4464=DIRECTION('ref_axis',(0.,0.,-1.));
#4465=DIRECTION('center_axis',(0.,0.,1.));
#4466=DIRECTION('ref_axis',(1.,0.,0.));
#4467=DIRECTION('center_axis',(0.,0.,1.));
#4468=DIRECTION('ref_axis',(1.,0.,0.));
#4469=DIRECTION('',(0.,0.,1.));
#4470=DIRECTION('center_axis',(0.,0.,1.));
#4471=DIRECTION('ref_axis',(1.,0.,0.));
#4472=DIRECTION('center_axis',(0.,0.,1.));
#4473=DIRECTION('ref_axis',(1.,0.,0.));
#4474=DIRECTION('',(0.,0.,1.));
#4475=DIRECTION('center_axis',(0.,1.,0.));
#4476=DIRECTION('ref_axis',(1.,0.,0.));
#4477=DIRECTION('center_axis',(0.,1.,0.));
#4478=DIRECTION('ref_axis',(1.,0.,0.));
#4479=DIRECTION('',(0.,1.,0.));
#4480=DIRECTION('center_axis',(0.,-1.,0.));
#4481=DIRECTION('ref_axis',(1.,0.,0.));
#4482=DIRECTION('center_axis',(0.,-1.,0.));
#4483=DIRECTION('ref_axis',(0.,0.,-1.));
#4484=DIRECTION('',(0.,0.,-1.));
#4485=DIRECTION('',(1.,0.,0.));
#4486=DIRECTION('',(0.,0.,1.));
#4487=DIRECTION('',(0.,0.,1.));
#4488=DIRECTION('',(-1.,0.,0.));
#4489=DIRECTION('',(0.,0.,-1.));
#4490=DIRECTION('',(-1.,0.,0.));
#4491=DIRECTION('',(0.,0.,1.));
#4492=DIRECTION('',(-1.,0.,0.));
#4493=DIRECTION('center_axis',(-1.,0.,0.));
#4494=DIRECTION('ref_axis',(0.,0.,1.));
#4495=DIRECTION('',(0.,0.,1.));
#4496=DIRECTION('',(0.,1.,0.));
#4497=DIRECTION('center_axis',(0.,0.,-1.));
#4498=DIRECTION('ref_axis',(-1.,0.,0.));
#4499=DIRECTION('',(-1.,0.,0.));
#4500=DIRECTION('',(0.,1.,0.));
#4501=DIRECTION('center_axis',(1.,0.,0.));
#4502=DIRECTION('ref_axis',(0.,0.,-1.));
#4503=DIRECTION('',(0.,0.,-1.));
#4504=DIRECTION('center_axis',(1.,0.,0.));
#4505=DIRECTION('ref_axis',(0.,0.,-1.));
#4506=DIRECTION('',(0.,0.,-1.));
#4507=DIRECTION('',(0.,1.,0.));
#4508=DIRECTION('center_axis',(0.,0.,1.));
#4509=DIRECTION('ref_axis',(1.,0.,0.));
#4510=DIRECTION('',(1.,0.,0.));
#4511=DIRECTION('',(0.,1.,0.));
#4512=DIRECTION('center_axis',(-1.,0.,0.));
#4513=DIRECTION('ref_axis',(0.,0.,1.));
#4514=DIRECTION('',(0.,0.,1.));
#4515=DIRECTION('',(0.,1.,0.));
#4516=DIRECTION('center_axis',(0.,0.,1.));
#4517=DIRECTION('ref_axis',(1.,0.,0.));
#4518=DIRECTION('',(1.,0.,0.));
#4519=DIRECTION('',(0.,1.,0.));
#4520=DIRECTION('center_axis',(1.,0.,0.));
#4521=DIRECTION('ref_axis',(0.,0.,-1.));
#4522=DIRECTION('',(0.,0.,-1.));
#4523=DIRECTION('',(0.,1.,0.));
#4524=DIRECTION('center_axis',(0.,0.,1.));
#4525=DIRECTION('ref_axis',(1.,0.,0.));
#4526=DIRECTION('',(1.,0.,0.));
#4527=DIRECTION('center_axis',(0.,1.,0.));
#4528=DIRECTION('ref_axis',(0.,0.,1.));
#4529=DIRECTION('axis',(0.,0.,1.));
#4530=DIRECTION('refdir',(1.,0.,0.));
#4531=DIRECTION('center_axis',(0.866025403784439,0.,-0.5));
#4532=DIRECTION('ref_axis',(0.5,0.,0.866025403784439));
#4533=DIRECTION('',(-0.5,0.,-0.866025403784439));
#4534=DIRECTION('',(0.,-1.,0.));
#4535=DIRECTION('',(0.5,0.,0.866025403784439));
#4536=DIRECTION('',(0.,-1.,0.));
#4537=DIRECTION('center_axis',(1.20185167898973E-16,0.,-1.));
#4538=DIRECTION('ref_axis',(1.,0.,1.20185167898973E-16));
#4539=DIRECTION('',(-1.,0.,-1.20185167898973E-16));
#4540=DIRECTION('',(0.,-1.,0.));
#4541=DIRECTION('',(1.,0.,1.20185167898973E-16));
#4542=DIRECTION('center_axis',(-0.866025403784439,0.,-0.5));
#4543=DIRECTION('ref_axis',(0.5,0.,-0.866025403784439));
#4544=DIRECTION('',(-0.5,0.,0.866025403784439));
#4545=DIRECTION('',(0.,-1.,0.));
#4546=DIRECTION('',(0.5,0.,-0.866025403784439));
#4547=DIRECTION('center_axis',(-0.866025403784439,0.,0.5));
#4548=DIRECTION('ref_axis',(-0.5,0.,-0.866025403784439));
#4549=DIRECTION('',(0.5,0.,0.866025403784439));
#4550=DIRECTION('',(0.,-1.,0.));
#4551=DIRECTION('',(-0.5,0.,-0.866025403784439));
#4552=DIRECTION('center_axis',(-2.40370335797945E-16,0.,1.));
#4553=DIRECTION('ref_axis',(-1.,0.,-2.40370335797945E-16));
#4554=DIRECTION('',(1.,0.,2.40370335797945E-16));
#4555=DIRECTION('',(0.,-1.,0.));
#4556=DIRECTION('',(-1.,0.,-2.40370335797945E-16));
#4557=DIRECTION('center_axis',(0.866025403784439,0.,0.5));
#4558=DIRECTION('ref_axis',(-0.5,0.,0.866025403784439));
#4559=DIRECTION('',(0.5,0.,-0.866025403784439));
#4560=DIRECTION('',(-0.5,0.,0.866025403784439));
#4561=DIRECTION('center_axis',(0.,1.,0.));
#4562=DIRECTION('ref_axis',(1.,0.,0.));
#4563=DIRECTION('center_axis',(0.,-1.,0.));
#4564=DIRECTION('ref_axis',(0.,0.,-1.));
#4565=DIRECTION('center_axis',(0.,1.,0.));
#4566=DIRECTION('ref_axis',(1.,0.,0.));
#4567=DIRECTION('center_axis',(0.,1.,0.));
#4568=DIRECTION('ref_axis',(1.,0.,0.));
#4569=DIRECTION('center_axis',(0.,1.,0.));
#4570=DIRECTION('ref_axis',(0.,0.,1.));
#4571=DIRECTION('center_axis',(0.,-1.,0.));
#4572=DIRECTION('ref_axis',(1.,0.,0.));
#4573=DIRECTION('center_axis',(0.,-1.,0.));
#4574=DIRECTION('ref_axis',(1.,0.,0.));
#4575=DIRECTION('center_axis',(0.,-1.,0.));
#4576=DIRECTION('ref_axis',(1.,0.,0.));
#4577=DIRECTION('',(0.707106781186548,0.707106781186547,8.65956056235493E-17));
#4578=DIRECTION('center_axis',(0.,-1.,0.));
#4579=DIRECTION('ref_axis',(1.,0.,0.));
#4580=DIRECTION('center_axis',(0.,-1.,0.));
#4581=DIRECTION('ref_axis',(1.,0.,0.));
#4582=DIRECTION('',(0.,1.,0.));
#4583=DIRECTION('center_axis',(0.,1.,0.));
#4584=DIRECTION('ref_axis',(1.,0.,0.));
#4585=DIRECTION('center_axis',(0.,-1.,0.));
#4586=DIRECTION('ref_axis',(1.,0.,0.));
#4587=DIRECTION('',(-0.707106781186547,0.707106781186548,-8.65956056235493E-17));
#4588=DIRECTION('center_axis',(0.,-1.,0.));
#4589=DIRECTION('ref_axis',(0.,0.,-1.));
#4590=DIRECTION('center_axis',(0.,-1.,0.));
#4591=DIRECTION('ref_axis',(1.,0.,0.));
#4592=DIRECTION('center_axis',(0.,1.,0.));
#4593=DIRECTION('ref_axis',(1.,0.,0.));
#4594=DIRECTION('center_axis',(0.,1.,0.));
#4595=DIRECTION('ref_axis',(1.,0.,0.));
#4596=DIRECTION('',(-0.447213595499958,0.894427190999916,-5.47678698264203E-17));
#4597=DIRECTION('center_axis',(0.,-1.,0.));
#4598=DIRECTION('ref_axis',(1.,0.,0.));
#4599=DIRECTION('',(0.,1.,0.));
#4600=DIRECTION('axis',(0.,0.,1.));
#4601=DIRECTION('refdir',(1.,0.,0.));
#4602=DIRECTION('center_axis',(0.,0.,1.));
#4603=DIRECTION('ref_axis',(1.,0.,0.));
#4604=DIRECTION('center_axis',(0.,0.,1.));
#4605=DIRECTION('ref_axis',(1.,0.,0.));
#4606=DIRECTION('',(0.,0.,1.));
#4607=DIRECTION('center_axis',(0.,0.,-1.));
#4608=DIRECTION('ref_axis',(1.,0.,0.));
#4609=DIRECTION('center_axis',(0.,0.,1.));
#4610=DIRECTION('ref_axis',(1.,0.,0.));
#4611=DIRECTION('center_axis',(0.,0.,1.));
#4612=DIRECTION('ref_axis',(1.,0.,0.));
#4613=DIRECTION('center_axis',(0.,0.,1.));
#4614=DIRECTION('ref_axis',(1.,0.,0.));
#4615=DIRECTION('center_axis',(0.,0.,1.));
#4616=DIRECTION('ref_axis',(1.,0.,0.));
#4617=DIRECTION('',(0.,0.,1.));
#4618=DIRECTION('center_axis',(0.,0.,-1.));
#4619=DIRECTION('ref_axis',(1.,0.,0.));
#4620=DIRECTION('center_axis',(0.,0.,1.));
#4621=DIRECTION('ref_axis',(1.,0.,0.));
#4622=DIRECTION('center_axis',(0.,0.,1.));
#4623=DIRECTION('ref_axis',(1.,0.,0.));
#4624=DIRECTION('center_axis',(0.,0.,1.));
#4625=DIRECTION('ref_axis',(1.,0.,0.));
#4626=DIRECTION('center_axis',(0.,0.,1.));
#4627=DIRECTION('ref_axis',(1.,0.,0.));
#4628=DIRECTION('',(0.,0.,1.));
#4629=DIRECTION('center_axis',(0.,0.,1.));
#4630=DIRECTION('ref_axis',(1.,0.,0.));
#4631=DIRECTION('center_axis',(0.,0.,1.));
#4632=DIRECTION('ref_axis',(1.,0.,0.));
#4633=DIRECTION('',(0.,0.,1.));
#4634=DIRECTION('center_axis',(0.,1.,0.));
#4635=DIRECTION('ref_axis',(-1.,0.,0.));
#4636=DIRECTION('',(-1.,0.,0.));
#4637=DIRECTION('',(0.,0.,1.));
#4638=DIRECTION('',(-1.,0.,0.));
#4639=DIRECTION('',(0.,0.,1.));
#4640=DIRECTION('center_axis',(1.,0.,0.));
#4641=DIRECTION('ref_axis',(0.,1.,0.));
#4642=DIRECTION('',(0.,1.,0.));
#4643=DIRECTION('',(0.,1.,0.));
#4644=DIRECTION('',(0.,0.,1.));
#4645=DIRECTION('center_axis',(0.,-1.,0.));
#4646=DIRECTION('ref_axis',(1.,0.,0.));
#4647=DIRECTION('',(1.,0.,0.));
#4648=DIRECTION('',(1.,0.,0.));
#4649=DIRECTION('',(0.,0.,1.));
#4650=DIRECTION('center_axis',(-1.,0.,0.));
#4651=DIRECTION('ref_axis',(0.,-1.,0.));
#4652=DIRECTION('',(0.,-1.,0.));
#4653=DIRECTION('',(0.,-1.,0.));
#4654=DIRECTION('center_axis',(0.,0.,1.));
#4655=DIRECTION('ref_axis',(1.,0.,0.));
#4656=DIRECTION('center_axis',(0.,0.,1.));
#4657=DIRECTION('ref_axis',(1.,0.,0.));
#4658=DIRECTION('axis',(0.,0.,1.));
#4659=DIRECTION('refdir',(1.,0.,0.));
#4660=DIRECTION('center_axis',(0.,1.,0.));
#4661=DIRECTION('ref_axis',(-1.,0.,0.));
#4662=DIRECTION('',(-1.,0.,0.));
#4663=DIRECTION('',(0.,0.,1.));
#4664=DIRECTION('',(-1.,0.,0.));
#4665=DIRECTION('',(0.,0.,1.));
#4666=DIRECTION('center_axis',(1.,0.,0.));
#4667=DIRECTION('ref_axis',(0.,1.,0.));
#4668=DIRECTION('',(0.,1.,0.));
#4669=DIRECTION('',(0.,1.,0.));
#4670=DIRECTION('',(0.,0.,1.));
#4671=DIRECTION('center_axis',(0.,-1.,0.));
#4672=DIRECTION('ref_axis',(1.,0.,0.));
#4673=DIRECTION('',(1.,0.,0.));
#4674=DIRECTION('',(1.,0.,0.));
#4675=DIRECTION('',(0.,0.,1.));
#4676=DIRECTION('center_axis',(-1.,0.,0.));
#4677=DIRECTION('ref_axis',(0.,-1.,0.));
#4678=DIRECTION('',(0.,-1.,0.));
#4679=DIRECTION('',(0.,-1.,0.));
#4680=DIRECTION('center_axis',(0.,0.,1.));
#4681=DIRECTION('ref_axis',(1.,0.,0.));
#4682=DIRECTION('center_axis',(0.,0.,1.));
#4683=DIRECTION('ref_axis',(1.,0.,0.));
#4684=DIRECTION('axis',(0.,0.,1.));
#4685=DIRECTION('refdir',(1.,0.,0.));
#4686=DIRECTION('axis',(0.,0.,1.));
#4687=DIRECTION('refdir',(1.,0.,0.));
#4688=DIRECTION('center_axis',(1.,0.,0.));
#4689=DIRECTION('ref_axis',(0.,0.,-1.));
#4690=DIRECTION('center_axis',(1.,0.,0.));
#4691=DIRECTION('ref_axis',(0.,0.,-1.));
#4692=DIRECTION('',(1.,0.,0.));
#4693=DIRECTION('center_axis',(-1.,0.,0.));
#4694=DIRECTION('ref_axis',(0.,0.,-1.));
#4695=DIRECTION('center_axis',(1.,0.,0.));
#4696=DIRECTION('ref_axis',(0.,0.,-1.));
#4697=DIRECTION('center_axis',(1.,0.,0.));
#4698=DIRECTION('ref_axis',(0.,0.,-1.));
#4699=DIRECTION('',(1.,0.,0.));
#4700=DIRECTION('center_axis',(-1.,0.,0.));
#4701=DIRECTION('ref_axis',(0.,0.,-1.));
#4702=DIRECTION('center_axis',(1.,0.,0.));
#4703=DIRECTION('ref_axis',(0.,0.,-1.));
#4704=DIRECTION('center_axis',(1.,0.,0.));
#4705=DIRECTION('ref_axis',(0.,0.,-1.));
#4706=DIRECTION('',(1.,0.,0.));
#4707=DIRECTION('center_axis',(-1.,0.,0.));
#4708=DIRECTION('ref_axis',(0.,0.,-1.));
#4709=DIRECTION('center_axis',(1.,0.,0.));
#4710=DIRECTION('ref_axis',(0.,0.,-1.));
#4711=DIRECTION('center_axis',(1.,0.,0.));
#4712=DIRECTION('ref_axis',(0.,0.,-1.));
#4713=DIRECTION('',(1.,0.,0.));
#4714=DIRECTION('center_axis',(-1.,0.,0.));
#4715=DIRECTION('ref_axis',(0.,0.,-1.));
#4716=DIRECTION('center_axis',(0.,0.,1.));
#4717=DIRECTION('ref_axis',(1.,0.,0.));
#4718=DIRECTION('center_axis',(0.,0.,1.));
#4719=DIRECTION('ref_axis',(1.,0.,0.));
#4720=DIRECTION('',(0.,0.,1.));
#4721=DIRECTION('center_axis',(0.,0.,-1.));
#4722=DIRECTION('ref_axis',(1.,0.,0.));
#4723=DIRECTION('center_axis',(0.,0.,1.));
#4724=DIRECTION('ref_axis',(1.,0.,0.));
#4725=DIRECTION('center_axis',(0.,0.,1.));
#4726=DIRECTION('ref_axis',(1.,0.,0.));
#4727=DIRECTION('center_axis',(0.,0.,1.));
#4728=DIRECTION('ref_axis',(1.,0.,0.));
#4729=DIRECTION('',(0.,0.,1.));
#4730=DIRECTION('center_axis',(0.,0.,-1.));
#4731=DIRECTION('ref_axis',(1.,0.,0.));
#4732=DIRECTION('center_axis',(0.,0.,1.));
#4733=DIRECTION('ref_axis',(1.,0.,0.));
#4734=DIRECTION('center_axis',(0.,0.,1.));
#4735=DIRECTION('ref_axis',(1.,0.,0.));
#4736=DIRECTION('center_axis',(0.,0.,1.));
#4737=DIRECTION('ref_axis',(1.,0.,0.));
#4738=DIRECTION('',(0.,0.,1.));
#4739=DIRECTION('center_axis',(0.,0.,-1.));
#4740=DIRECTION('ref_axis',(1.,0.,0.));
#4741=DIRECTION('center_axis',(0.,0.,1.));
#4742=DIRECTION('ref_axis',(1.,0.,0.));
#4743=DIRECTION('center_axis',(0.,0.,1.));
#4744=DIRECTION('ref_axis',(1.,0.,0.));
#4745=DIRECTION('center_axis',(0.,0.,1.));
#4746=DIRECTION('ref_axis',(1.,0.,0.));
#4747=DIRECTION('',(0.,0.,1.));
#4748=DIRECTION('center_axis',(0.,0.,-1.));
#4749=DIRECTION('ref_axis',(1.,0.,0.));
#4750=DIRECTION('center_axis',(0.,0.,1.));
#4751=DIRECTION('ref_axis',(1.,0.,0.));
#4752=DIRECTION('center_axis',(1.,0.,0.));
#4753=DIRECTION('ref_axis',(0.,0.,-1.));
#4754=DIRECTION('center_axis',(1.,0.,0.));
#4755=DIRECTION('ref_axis',(0.,0.,-1.));
#4756=DIRECTION('',(1.,0.,0.));
#4757=DIRECTION('center_axis',(-1.,0.,0.));
#4758=DIRECTION('ref_axis',(0.,0.,-1.));
#4759=DIRECTION('center_axis',(1.,0.,0.));
#4760=DIRECTION('ref_axis',(0.,0.,-1.));
#4761=DIRECTION('center_axis',(1.,0.,0.));
#4762=DIRECTION('ref_axis',(0.,0.,-1.));
#4763=DIRECTION('',(1.,0.,0.));
#4764=DIRECTION('center_axis',(-1.,0.,0.));
#4765=DIRECTION('ref_axis',(0.,0.,-1.));
#4766=DIRECTION('center_axis',(0.,1.,0.));
#4767=DIRECTION('ref_axis',(-1.,0.,0.));
#4768=DIRECTION('',(-1.,0.,0.));
#4769=DIRECTION('',(0.,0.,1.));
#4770=DIRECTION('',(-1.,0.,0.));
#4771=DIRECTION('',(0.,0.,1.));
#4772=DIRECTION('center_axis',(1.,0.,0.));
#4773=DIRECTION('ref_axis',(0.,1.,0.));
#4774=DIRECTION('',(0.,1.,0.));
#4775=DIRECTION('',(0.,1.,0.));
#4776=DIRECTION('',(0.,0.,1.));
#4777=DIRECTION('center_axis',(0.,-1.,0.));
#4778=DIRECTION('ref_axis',(1.,0.,0.));
#4779=DIRECTION('',(1.,0.,0.));
#4780=DIRECTION('',(1.,0.,0.));
#4781=DIRECTION('',(0.,0.,1.));
#4782=DIRECTION('center_axis',(-1.,0.,0.));
#4783=DIRECTION('ref_axis',(0.,-1.,0.));
#4784=DIRECTION('',(0.,-1.,0.));
#4785=DIRECTION('',(0.,-1.,0.));
#4786=DIRECTION('center_axis',(0.,0.,1.));
#4787=DIRECTION('ref_axis',(1.,0.,0.));
#4788=DIRECTION('center_axis',(0.,0.,1.));
#4789=DIRECTION('ref_axis',(1.,0.,0.));
#4790=DIRECTION('axis',(0.,0.,1.));
#4791=DIRECTION('refdir',(1.,0.,0.));
#4792=DIRECTION('center_axis',(0.,0.,1.));
#4793=DIRECTION('ref_axis',(1.,0.,0.));
#4794=DIRECTION('center_axis',(0.,0.,1.));
#4795=DIRECTION('ref_axis',(1.,0.,0.));
#4796=DIRECTION('',(0.,0.,1.));
#4797=DIRECTION('center_axis',(0.,0.,-1.));
#4798=DIRECTION('ref_axis',(1.,0.,0.));
#4799=DIRECTION('center_axis',(0.,0.,1.));
#4800=DIRECTION('ref_axis',(1.,0.,0.));
#4801=DIRECTION('center_axis',(0.,0.,1.));
#4802=DIRECTION('ref_axis',(1.,0.,0.));
#4803=DIRECTION('',(0.,0.,1.));
#4804=DIRECTION('center_axis',(0.,0.,-1.));
#4805=DIRECTION('ref_axis',(1.,0.,0.));
#4806=DIRECTION('center_axis',(0.,0.,1.));
#4807=DIRECTION('ref_axis',(1.,0.,0.));
#4808=DIRECTION('center_axis',(0.,0.,1.));
#4809=DIRECTION('ref_axis',(1.,0.,0.));
#4810=DIRECTION('',(0.,0.,1.));
#4811=DIRECTION('center_axis',(0.,0.,-1.));
#4812=DIRECTION('ref_axis',(1.,0.,0.));
#4813=DIRECTION('center_axis',(0.,0.,1.));
#4814=DIRECTION('ref_axis',(1.,0.,0.));
#4815=DIRECTION('center_axis',(0.,0.,1.));
#4816=DIRECTION('ref_axis',(1.,0.,0.));
#4817=DIRECTION('',(0.,0.,1.));
#4818=DIRECTION('center_axis',(0.,0.,-1.));
#4819=DIRECTION('ref_axis',(1.,0.,0.));
#4820=DIRECTION('center_axis',(0.,0.,1.));
#4821=DIRECTION('ref_axis',(1.,0.,0.));
#4822=DIRECTION('center_axis',(0.,0.,1.));
#4823=DIRECTION('ref_axis',(1.,0.,0.));
#4824=DIRECTION('',(0.,0.,1.));
#4825=DIRECTION('center_axis',(0.,0.,-1.));
#4826=DIRECTION('ref_axis',(1.,0.,0.));
#4827=DIRECTION('center_axis',(0.,1.,0.));
#4828=DIRECTION('ref_axis',(-1.,0.,0.));
#4829=DIRECTION('',(-1.,0.,0.));
#4830=DIRECTION('',(0.,0.,1.));
#4831=DIRECTION('',(-1.,0.,0.));
#4832=DIRECTION('',(0.,0.,1.));
#4833=DIRECTION('center_axis',(1.,0.,0.));
#4834=DIRECTION('ref_axis',(0.,1.,0.));
#4835=DIRECTION('',(0.,1.,0.));
#4836=DIRECTION('',(0.,1.,0.));
#4837=DIRECTION('',(0.,0.,1.));
#4838=DIRECTION('center_axis',(0.,-1.,0.));
#4839=DIRECTION('ref_axis',(1.,0.,0.));
#4840=DIRECTION('',(1.,0.,0.));
#4841=DIRECTION('',(1.,0.,0.));
#4842=DIRECTION('',(0.,0.,1.));
#4843=DIRECTION('center_axis',(-1.,0.,0.));
#4844=DIRECTION('ref_axis',(0.,-1.,0.));
#4845=DIRECTION('',(0.,-1.,0.));
#4846=DIRECTION('',(0.,-1.,0.));
#4847=DIRECTION('center_axis',(0.,0.,1.));
#4848=DIRECTION('ref_axis',(1.,0.,0.));
#4849=DIRECTION('center_axis',(0.,0.,1.));
#4850=DIRECTION('ref_axis',(1.,0.,0.));
#4851=DIRECTION('axis',(0.,0.,1.));
#4852=DIRECTION('refdir',(1.,0.,0.));
#4853=DIRECTION('axis',(0.,0.,1.));
#4854=DIRECTION('refdir',(1.,0.,0.));
#4855=DIRECTION('center_axis',(0.,1.,0.));
#4856=DIRECTION('ref_axis',(0.,0.,1.));
#4857=DIRECTION('center_axis',(0.,-1.,0.));
#4858=DIRECTION('ref_axis',(1.,0.,0.));
#4859=DIRECTION('',(-1.,0.,0.));
#4860=DIRECTION('',(0.,0.,-1.));
#4861=DIRECTION('',(1.,0.,0.));
#4862=DIRECTION('center_axis',(0.,0.,1.));
#4863=DIRECTION('ref_axis',(1.,0.,0.));
#4864=DIRECTION('',(0.,-1.,0.));
#4865=DIRECTION('',(0.,1.,0.));
#4866=DIRECTION('',(-1.,0.,0.));
#4867=DIRECTION('center_axis',(0.,-1.,0.));
#4868=DIRECTION('ref_axis',(0.,0.,-1.));
#4869=DIRECTION('center_axis',(0.,1.,0.));
#4870=DIRECTION('ref_axis',(1.,0.,0.));
#4871=DIRECTION('',(0.,0.,1.));
#4872=DIRECTION('',(1.,0.,0.));
#4873=DIRECTION('center_axis',(0.,0.,-1.));
#4874=DIRECTION('ref_axis',(-1.,0.,0.));
#4875=DIRECTION('',(0.,1.,0.));
#4876=DIRECTION('',(0.,1.,0.));
#4877=DIRECTION('center_axis',(1.,0.,0.));
#4878=DIRECTION('ref_axis',(0.,0.,-1.));
#4879=DIRECTION('center_axis',(0.,1.,0.));
#4880=DIRECTION('ref_axis',(0.,0.,1.));
#4881=DIRECTION('center_axis',(0.,-1.,0.));
#4882=DIRECTION('ref_axis',(1.,0.,0.));
#4883=DIRECTION('center_axis',(0.,-1.,0.));
#4884=DIRECTION('ref_axis',(1.,0.,0.));
#4885=DIRECTION('center_axis',(0.,-1.,0.));
#4886=DIRECTION('ref_axis',(1.,0.,0.));
#4887=DIRECTION('center_axis',(0.,-1.,0.));
#4888=DIRECTION('ref_axis',(1.,0.,0.));
#4889=DIRECTION('',(0.,1.,0.));
#4890=DIRECTION('center_axis',(0.,-1.,0.));
#4891=DIRECTION('ref_axis',(0.,0.,-1.));
#4892=DIRECTION('center_axis',(0.,-1.,0.));
#4893=DIRECTION('ref_axis',(1.,0.,0.));
#4894=DIRECTION('center_axis',(0.,-1.,0.));
#4895=DIRECTION('ref_axis',(1.,0.,0.));
#4896=DIRECTION('center_axis',(0.,-1.,0.));
#4897=DIRECTION('ref_axis',(1.,0.,0.));
#4898=DIRECTION('',(0.,1.,0.));
#4899=DIRECTION('center_axis',(0.,1.,0.));
#4900=DIRECTION('ref_axis',(0.,0.,1.));
#4901=DIRECTION('center_axis',(0.,-1.,0.));
#4902=DIRECTION('ref_axis',(1.,0.,0.));
#4903=DIRECTION('center_axis',(0.,-1.,0.));
#4904=DIRECTION('ref_axis',(1.,0.,0.));
#4905=DIRECTION('center_axis',(0.,-1.,0.));
#4906=DIRECTION('ref_axis',(1.,0.,0.));
#4907=DIRECTION('',(0.,1.,0.));
#4908=DIRECTION('center_axis',(0.,-1.,0.));
#4909=DIRECTION('ref_axis',(0.,0.,-1.));
#4910=DIRECTION('center_axis',(0.,-1.,0.));
#4911=DIRECTION('ref_axis',(1.,0.,0.));
#4912=DIRECTION('center_axis',(0.,-1.,0.));
#4913=DIRECTION('ref_axis',(1.,0.,0.));
#4914=DIRECTION('center_axis',(0.,-1.,0.));
#4915=DIRECTION('ref_axis',(1.,0.,0.));
#4916=DIRECTION('',(0.,1.,0.));
#4917=DIRECTION('center_axis',(0.,1.,0.));
#4918=DIRECTION('ref_axis',(0.,0.,1.));
#4919=DIRECTION('center_axis',(0.,-1.,0.));
#4920=DIRECTION('ref_axis',(1.,0.,0.));
#4921=DIRECTION('center_axis',(0.,-1.,0.));
#4922=DIRECTION('ref_axis',(1.,0.,0.));
#4923=DIRECTION('center_axis',(0.,-1.,0.));
#4924=DIRECTION('ref_axis',(1.,0.,0.));
#4925=DIRECTION('',(0.,1.,0.));
#4926=DIRECTION('center_axis',(0.,-1.,0.));
#4927=DIRECTION('ref_axis',(0.,0.,-1.));
#4928=DIRECTION('center_axis',(0.,-1.,0.));
#4929=DIRECTION('ref_axis',(1.,0.,0.));
#4930=DIRECTION('center_axis',(0.,-1.,0.));
#4931=DIRECTION('ref_axis',(1.,0.,0.));
#4932=DIRECTION('',(0.,1.,0.));
#4933=DIRECTION('axis',(0.,0.,1.));
#4934=DIRECTION('refdir',(1.,0.,0.));
#4935=DIRECTION('center_axis',(0.,1.,0.));
#4936=DIRECTION('ref_axis',(0.,0.,1.));
#4937=DIRECTION('center_axis',(0.,1.,0.));
#4938=DIRECTION('ref_axis',(1.,0.,0.));
#4939=DIRECTION('',(1.,0.,0.));
#4940=DIRECTION('center_axis',(0.,-1.,0.));
#4941=DIRECTION('ref_axis',(1.,0.,0.));
#4942=DIRECTION('',(-1.,0.,0.));
#4943=DIRECTION('center_axis',(0.,0.,-1.));
#4944=DIRECTION('ref_axis',(-1.,0.,0.));
#4945=DIRECTION('',(0.,-1.,0.));
#4946=DIRECTION('',(0.,1.,0.));
#4947=DIRECTION('',(1.,0.,0.));
#4948=DIRECTION('center_axis',(0.,-1.,0.));
#4949=DIRECTION('ref_axis',(0.,0.,-1.));
#4950=DIRECTION('center_axis',(0.,-1.,0.));
#4951=DIRECTION('ref_axis',(1.,0.,0.));
#4952=DIRECTION('center_axis',(0.,1.,0.));
#4953=DIRECTION('ref_axis',(1.,0.,0.));
#4954=DIRECTION('',(-1.,0.,0.));
#4955=DIRECTION('center_axis',(0.,0.,1.));
#4956=DIRECTION('ref_axis',(1.,0.,0.));
#4957=DIRECTION('',(0.,1.,0.));
#4958=DIRECTION('',(0.,-1.,0.));
#4959=DIRECTION('center_axis',(0.,1.,0.));
#4960=DIRECTION('ref_axis',(0.,0.,1.));
#4961=DIRECTION('center_axis',(0.,-1.,0.));
#4962=DIRECTION('ref_axis',(1.,0.,0.));
#4963=DIRECTION('center_axis',(0.,-1.,0.));
#4964=DIRECTION('ref_axis',(1.,0.,0.));
#4965=DIRECTION('center_axis',(0.,-1.,0.));
#4966=DIRECTION('ref_axis',(1.,0.,0.));
#4967=DIRECTION('center_axis',(0.,-1.,0.));
#4968=DIRECTION('ref_axis',(1.,0.,0.));
#4969=DIRECTION('',(0.,1.,0.));
#4970=DIRECTION('center_axis',(0.,-1.,0.));
#4971=DIRECTION('ref_axis',(0.,0.,-1.));
#4972=DIRECTION('center_axis',(0.,-1.,0.));
#4973=DIRECTION('ref_axis',(1.,0.,0.));
#4974=DIRECTION('center_axis',(0.,-1.,0.));
#4975=DIRECTION('ref_axis',(1.,0.,0.));
#4976=DIRECTION('',(0.,1.,0.));
#4977=DIRECTION('',(0.,0.,1.));
#4978=DIRECTION('',(1.,0.,0.));
#4979=DIRECTION('',(0.,0.,1.));
#4980=DIRECTION('',(1.,0.,0.));
#4981=DIRECTION('axis',(0.,0.,1.));
#4982=DIRECTION('refdir',(1.,0.,0.));
#4983=DIRECTION('center_axis',(1.,0.,0.));
#4984=DIRECTION('ref_axis',(0.,0.,-1.));
#4985=DIRECTION('center_axis',(1.,0.,0.));
#4986=DIRECTION('ref_axis',(0.,0.,-1.));
#4987=DIRECTION('',(1.,0.,0.));
#4988=DIRECTION('center_axis',(-1.,0.,0.));
#4989=DIRECTION('ref_axis',(0.,0.,-1.));
#4990=DIRECTION('center_axis',(1.,0.,0.));
#4991=DIRECTION('ref_axis',(0.,0.,-1.));
#4992=DIRECTION('center_axis',(1.,0.,0.));
#4993=DIRECTION('ref_axis',(0.,0.,-1.));
#4994=DIRECTION('',(1.,0.,0.));
#4995=DIRECTION('center_axis',(-1.,0.,0.));
#4996=DIRECTION('ref_axis',(0.,0.,-1.));
#4997=DIRECTION('center_axis',(1.,0.,0.));
#4998=DIRECTION('ref_axis',(0.,0.,-1.));
#4999=DIRECTION('center_axis',(1.,0.,0.));
#5000=DIRECTION('ref_axis',(0.,0.,-1.));
#5001=DIRECTION('',(1.,0.,0.));
#5002=DIRECTION('center_axis',(-1.,0.,0.));
#5003=DIRECTION('ref_axis',(0.,0.,-1.));
#5004=DIRECTION('center_axis',(1.,0.,0.));
#5005=DIRECTION('ref_axis',(0.,0.,-1.));
#5006=DIRECTION('center_axis',(1.,0.,0.));
#5007=DIRECTION('ref_axis',(0.,0.,-1.));
#5008=DIRECTION('',(1.,0.,0.));
#5009=DIRECTION('center_axis',(-1.,0.,0.));
#5010=DIRECTION('ref_axis',(0.,0.,-1.));
#5011=DIRECTION('center_axis',(1.,0.,0.));
#5012=DIRECTION('ref_axis',(0.,0.,-1.));
#5013=DIRECTION('center_axis',(1.,0.,0.));
#5014=DIRECTION('ref_axis',(0.,0.,-1.));
#5015=DIRECTION('',(1.,0.,0.));
#5016=DIRECTION('center_axis',(-1.,0.,0.));
#5017=DIRECTION('ref_axis',(0.,0.,-1.));
#5018=DIRECTION('center_axis',(1.,0.,0.));
#5019=DIRECTION('ref_axis',(0.,0.,-1.));
#5020=DIRECTION('center_axis',(1.,0.,0.));
#5021=DIRECTION('ref_axis',(0.,0.,-1.));
#5022=DIRECTION('',(1.,0.,0.));
#5023=DIRECTION('center_axis',(-1.,0.,0.));
#5024=DIRECTION('ref_axis',(0.,0.,-1.));
#5025=DIRECTION('center_axis',(0.,1.,0.));
#5026=DIRECTION('ref_axis',(-1.,0.,0.));
#5027=DIRECTION('',(-1.,0.,0.));
#5028=DIRECTION('',(0.,0.,1.));
#5029=DIRECTION('',(-1.,0.,0.));
#5030=DIRECTION('',(0.,0.,1.));
#5031=DIRECTION('center_axis',(1.,0.,0.));
#5032=DIRECTION('ref_axis',(0.,1.,0.));
#5033=DIRECTION('',(0.,1.,0.));
#5034=DIRECTION('',(0.,1.,0.));
#5035=DIRECTION('',(0.,0.,1.));
#5036=DIRECTION('center_axis',(0.,-1.,0.));
#5037=DIRECTION('ref_axis',(1.,0.,0.));
#5038=DIRECTION('',(1.,0.,0.));
#5039=DIRECTION('',(1.,0.,0.));
#5040=DIRECTION('',(0.,0.,1.));
#5041=DIRECTION('center_axis',(-1.,0.,0.));
#5042=DIRECTION('ref_axis',(0.,-1.,0.));
#5043=DIRECTION('',(0.,-1.,0.));
#5044=DIRECTION('',(0.,-1.,0.));
#5045=DIRECTION('center_axis',(0.,0.,1.));
#5046=DIRECTION('ref_axis',(1.,0.,0.));
#5047=DIRECTION('center_axis',(0.,0.,1.));
#5048=DIRECTION('ref_axis',(1.,0.,0.));
#5049=DIRECTION('axis',(0.,0.,1.));
#5050=DIRECTION('refdir',(1.,0.,0.));
#5051=DIRECTION('center_axis',(0.,1.,0.));
#5052=DIRECTION('ref_axis',(0.,0.,1.));
#5053=DIRECTION('center_axis',(0.,-1.,0.));
#5054=DIRECTION('ref_axis',(1.,0.,0.));
#5055=DIRECTION('center_axis',(0.,-1.,0.));
#5056=DIRECTION('ref_axis',(1.,0.,0.));
#5057=DIRECTION('center_axis',(0.,-1.,0.));
#5058=DIRECTION('ref_axis',(1.,0.,0.));
#5059=DIRECTION('',(0.707106781186547,0.707106781186548,8.65956056235493E-17));
#5060=DIRECTION('center_axis',(0.,-1.,0.));
#5061=DIRECTION('ref_axis',(1.,0.,0.));
#5062=DIRECTION('center_axis',(0.,-1.,0.));
#5063=DIRECTION('ref_axis',(1.,0.,0.));
#5064=DIRECTION('',(0.,1.,0.));
#5065=DIRECTION('center_axis',(0.,1.,0.));
#5066=DIRECTION('ref_axis',(1.,0.,0.));
#5067=DIRECTION('center_axis',(0.,-1.,0.));
#5068=DIRECTION('ref_axis',(1.,0.,0.));
#5069=DIRECTION('',(-0.707106781186547,0.707106781186548,-8.65956056235493E-17));
#5070=DIRECTION('center_axis',(0.,-1.,0.));
#5071=DIRECTION('ref_axis',(0.,0.,-1.));
#5072=DIRECTION('center_axis',(0.,-1.,0.));
#5073=DIRECTION('ref_axis',(1.,0.,0.));
#5074=DIRECTION('center_axis',(0.,1.,0.));
#5075=DIRECTION('ref_axis',(1.,0.,0.));
#5076=DIRECTION('center_axis',(0.,1.,0.));
#5077=DIRECTION('ref_axis',(1.,0.,0.));
#5078=DIRECTION('',(-0.447213595499958,0.894427190999916,-5.47678698264203E-17));
#5079=DIRECTION('center_axis',(0.,-1.,0.));
#5080=DIRECTION('ref_axis',(1.,0.,0.));
#5081=DIRECTION('center_axis',(0.,1.,0.));
#5082=DIRECTION('ref_axis',(1.,0.,0.));
#5083=DIRECTION('',(0.,1.,0.));
#5084=DIRECTION('center_axis',(0.,1.,0.));
#5085=DIRECTION('ref_axis',(1.,0.,0.));
#5086=DIRECTION('center_axis',(0.,-1.,0.));
#5087=DIRECTION('ref_axis',(1.,0.,0.));
#5088=DIRECTION('',(-0.707106781186547,0.707106781186548,-8.65956056235493E-17));
#5089=DIRECTION('center_axis',(0.,-1.,0.));
#5090=DIRECTION('ref_axis',(0.,0.,-1.));
#5091=DIRECTION('center_axis',(0.866025403784439,0.,-0.5));
#5092=DIRECTION('ref_axis',(0.5,0.,0.866025403784439));
#5093=DIRECTION('',(-0.5,0.,-0.866025403784439));
#5094=DIRECTION('',(0.,-1.,0.));
#5095=DIRECTION('',(0.5,0.,0.866025403784439));
#5096=DIRECTION('',(0.,-1.,0.));
#5097=DIRECTION('center_axis',(1.60246890531964E-16,0.,-1.));
#5098=DIRECTION('ref_axis',(1.,0.,1.60246890531964E-16));
#5099=DIRECTION('',(-1.,0.,-1.60246890531964E-16));
#5100=DIRECTION('',(0.,-1.,0.));
#5101=DIRECTION('',(1.,0.,1.60246890531964E-16));
#5102=DIRECTION('center_axis',(-0.866025403784439,0.,-0.5));
#5103=DIRECTION('ref_axis',(0.5,0.,-0.866025403784439));
#5104=DIRECTION('',(-0.5,0.,0.866025403784439));
#5105=DIRECTION('',(0.,-1.,0.));
#5106=DIRECTION('',(0.5,0.,-0.866025403784439));
#5107=DIRECTION('center_axis',(-0.866025403784439,0.,0.5));
#5108=DIRECTION('ref_axis',(-0.5,0.,-0.866025403784439));
#5109=DIRECTION('',(0.5,0.,0.866025403784439));
#5110=DIRECTION('',(0.,-1.,0.));
#5111=DIRECTION('',(-0.5,0.,-0.866025403784439));
#5112=DIRECTION('center_axis',(-1.60246890531964E-16,0.,1.));
#5113=DIRECTION('ref_axis',(-1.,0.,-1.60246890531964E-16));
#5114=DIRECTION('',(1.,0.,1.60246890531964E-16));
#5115=DIRECTION('',(0.,-1.,0.));
#5116=DIRECTION('',(-1.,0.,-1.60246890531964E-16));
#5117=DIRECTION('center_axis',(0.866025403784439,0.,0.5));
#5118=DIRECTION('ref_axis',(-0.5,0.,0.866025403784439));
#5119=DIRECTION('',(0.5,0.,-0.866025403784439));
#5120=DIRECTION('',(-0.5,0.,0.866025403784439));
#5121=DIRECTION('center_axis',(0.,1.,0.));
#5122=DIRECTION('ref_axis',(1.,0.,0.));
#5123=DIRECTION('center_axis',(0.,-1.,0.));
#5124=DIRECTION('ref_axis',(0.,0.,-1.));
#5125=DIRECTION('axis',(0.,0.,1.));
#5126=DIRECTION('refdir',(1.,0.,0.));
#5127=DIRECTION('center_axis',(0.,1.,0.));
#5128=DIRECTION('ref_axis',(0.,0.,1.));
#5129=DIRECTION('center_axis',(0.,-1.,0.));
#5130=DIRECTION('ref_axis',(1.,0.,0.));
#5131=DIRECTION('center_axis',(0.,-1.,0.));
#5132=DIRECTION('ref_axis',(1.,0.,0.));
#5133=DIRECTION('center_axis',(0.,-1.,0.));
#5134=DIRECTION('ref_axis',(1.,0.,0.));
#5135=DIRECTION('',(0.707106781186548,0.707106781186547,8.65956056235493E-17));
#5136=DIRECTION('center_axis',(0.,-1.,0.));
#5137=DIRECTION('ref_axis',(1.,0.,0.));
#5138=DIRECTION('center_axis',(0.,-1.,0.));
#5139=DIRECTION('ref_axis',(1.,0.,0.));
#5140=DIRECTION('',(0.,1.,0.));
#5141=DIRECTION('center_axis',(0.,1.,0.));
#5142=DIRECTION('ref_axis',(1.,0.,0.));
#5143=DIRECTION('center_axis',(0.,-1.,0.));
#5144=DIRECTION('ref_axis',(1.,0.,0.));
#5145=DIRECTION('',(-0.707106781186547,0.707106781186548,-8.65956056235493E-17));
#5146=DIRECTION('center_axis',(0.,-1.,0.));
#5147=DIRECTION('ref_axis',(0.,0.,-1.));
#5148=DIRECTION('center_axis',(0.,-1.,0.));
#5149=DIRECTION('ref_axis',(1.,0.,0.));
#5150=DIRECTION('center_axis',(0.,1.,0.));
#5151=DIRECTION('ref_axis',(1.,0.,0.));
#5152=DIRECTION('center_axis',(0.,1.,0.));
#5153=DIRECTION('ref_axis',(1.,0.,0.));
#5154=DIRECTION('',(-0.447213595499958,0.894427190999916,-5.47678698264203E-17));
#5155=DIRECTION('center_axis',(0.,-1.,0.));
#5156=DIRECTION('ref_axis',(1.,0.,0.));
#5157=DIRECTION('center_axis',(0.,1.,0.));
#5158=DIRECTION('ref_axis',(1.,0.,0.));
#5159=DIRECTION('',(0.,1.,0.));
#5160=DIRECTION('center_axis',(0.,1.,0.));
#5161=DIRECTION('ref_axis',(1.,0.,0.));
#5162=DIRECTION('center_axis',(0.,-1.,0.));
#5163=DIRECTION('ref_axis',(1.,0.,0.));
#5164=DIRECTION('',(-0.707106781186547,0.707106781186548,-8.65956056235493E-17));
#5165=DIRECTION('center_axis',(0.,-1.,0.));
#5166=DIRECTION('ref_axis',(0.,0.,-1.));
#5167=DIRECTION('center_axis',(0.866025403784439,0.,-0.5));
#5168=DIRECTION('ref_axis',(0.5,0.,0.866025403784439));
#5169=DIRECTION('',(-0.5,0.,-0.866025403784439));
#5170=DIRECTION('',(0.,-1.,0.));
#5171=DIRECTION('',(0.5,0.,0.866025403784439));
#5172=DIRECTION('',(0.,-1.,0.));
#5173=DIRECTION('center_axis',(1.20185167898973E-16,0.,-1.));
#5174=DIRECTION('ref_axis',(1.,0.,1.20185167898973E-16));
#5175=DIRECTION('',(-1.,0.,-1.20185167898973E-16));
#5176=DIRECTION('',(0.,-1.,0.));
#5177=DIRECTION('',(1.,0.,1.20185167898973E-16));
#5178=DIRECTION('center_axis',(-0.866025403784439,0.,-0.5));
#5179=DIRECTION('ref_axis',(0.5,0.,-0.866025403784439));
#5180=DIRECTION('',(-0.5,0.,0.866025403784439));
#5181=DIRECTION('',(0.,-1.,0.));
#5182=DIRECTION('',(0.5,0.,-0.866025403784439));
#5183=DIRECTION('center_axis',(-0.866025403784439,0.,0.5));
#5184=DIRECTION('ref_axis',(-0.5,0.,-0.866025403784439));
#5185=DIRECTION('',(0.5,0.,0.866025403784439));
#5186=DIRECTION('',(0.,-1.,0.));
#5187=DIRECTION('',(-0.5,0.,-0.866025403784439));
#5188=DIRECTION('center_axis',(-2.40370335797945E-16,0.,1.));
#5189=DIRECTION('ref_axis',(-1.,0.,-2.40370335797945E-16));
#5190=DIRECTION('',(1.,0.,2.40370335797945E-16));
#5191=DIRECTION('',(0.,-1.,0.));
#5192=DIRECTION('',(-1.,0.,-2.40370335797945E-16));
#5193=DIRECTION('center_axis',(0.866025403784439,0.,0.5));
#5194=DIRECTION('ref_axis',(-0.5,0.,0.866025403784439));
#5195=DIRECTION('',(0.5,0.,-0.866025403784439));
#5196=DIRECTION('',(-0.5,0.,0.866025403784439));
#5197=DIRECTION('center_axis',(0.,1.,0.));
#5198=DIRECTION('ref_axis',(1.,0.,0.));
#5199=DIRECTION('center_axis',(0.,-1.,0.));
#5200=DIRECTION('ref_axis',(0.,0.,-1.));
#5201=DIRECTION('',(0.,0.,1.));
#5202=DIRECTION('',(1.,0.,0.));
#5203=DIRECTION('',(0.,0.,1.));
#5204=DIRECTION('',(1.,0.,0.));
#5205=DIRECTION('',(0.,0.,1.));
#5206=DIRECTION('',(2.22044604925031E-16,-1.,0.));
#5207=DIRECTION('',(0.,-1.,2.22044604925031E-16));
#5208=DIRECTION('',(1.,0.,0.));
#5209=DIRECTION('',(0.,-1.,2.22044604925031E-16));
#5210=DIRECTION('',(1.,0.,0.));
#5211=DIRECTION('',(0.,0.,1.));
#5212=DIRECTION('',(-1.,1.22464679914735E-16,0.));
#5213=DIRECTION('',(0.,0.,1.));
#5214=DIRECTION('',(2.22044604925031E-16,-1.,0.));
#5215=DIRECTION('',(0.,-1.,2.22044604925031E-16));
#5216=DIRECTION('',(1.,0.,0.));
#5217=DIRECTION('',(0.,-1.,2.22044604925031E-16));
#5218=DIRECTION('',(1.,0.,0.));
#5219=DIRECTION('',(0.,0.,1.));
#5220=DIRECTION('',(-1.,1.22464679914735E-16,0.));
#5221=DIRECTION('',(0.,0.,1.));
#5222=DIRECTION('',(1.,0.,0.));
#5223=DIRECTION('',(0.,0.,1.));
#5224=DIRECTION('',(2.22044604925031E-16,-1.,0.));
#5225=DIRECTION('',(0.,-1.,2.22044604925031E-16));
#5226=DIRECTION('',(1.,0.,0.));
#5227=DIRECTION('',(0.,-1.,2.22044604925031E-16));
#5228=DIRECTION('',(1.,0.,0.));
#5229=DIRECTION('',(0.,0.,1.));
#5230=DIRECTION('',(-1.,1.22464679914735E-16,0.));
#5231=DIRECTION('',(0.,0.,1.));
#5232=DIRECTION('',(2.22044604925031E-16,-1.,0.));
#5233=DIRECTION('',(0.,-1.,2.22044604925031E-16));
#5234=DIRECTION('',(1.,0.,0.));
#5235=DIRECTION('',(0.,-1.,2.22044604925031E-16));
#5236=DIRECTION('',(1.,0.,0.));
#5237=DIRECTION('',(0.,0.,1.));
#5238=DIRECTION('',(-1.,1.22464679914735E-16,0.));
#5239=DIRECTION('',(0.,0.,1.));
#5240=DIRECTION('',(1.,0.,0.));
#5241=DIRECTION('',(0.,-1.,2.22044604925031E-16));
#5242=DIRECTION('',(1.,0.,0.));
#5243=DIRECTION('',(0.,-1.,2.22044604925031E-16));
#5244=DIRECTION('',(1.,0.,0.));
#5245=DIRECTION('',(0.,0.,1.));
#5246=DIRECTION('',(1.,0.,0.));
#5247=DIRECTION('',(0.,-1.,2.22044604925031E-16));
#5248=DIRECTION('',(1.,0.,0.));
#5249=DIRECTION('',(0.,-1.,2.22044604925031E-16));
#5250=DIRECTION('',(1.,0.,0.));
#5251=DIRECTION('',(0.,0.,1.));
#5252=DIRECTION('',(1.,0.,0.));
#5253=DIRECTION('',(0.,0.,1.));
#5254=DIRECTION('',(1.,0.,0.));
#5255=DIRECTION('axis',(0.,0.,1.));
#5256=DIRECTION('refdir',(1.,0.,0.));
#5257=DIRECTION('center_axis',(0.,0.,1.));
#5258=DIRECTION('ref_axis',(1.,0.,0.));
#5259=DIRECTION('center_axis',(0.,0.,-1.));
#5260=DIRECTION('ref_axis',(1.,0.,0.));
#5261=DIRECTION('',(0.,0.,-1.));
#5262=DIRECTION('center_axis',(0.,0.,-1.));
#5263=DIRECTION('ref_axis',(1.,0.,0.));
#5264=DIRECTION('center_axis',(0.,0.,1.));
#5265=DIRECTION('ref_axis',(1.,0.,0.));
#5266=DIRECTION('center_axis',(0.,0.,1.));
#5267=DIRECTION('ref_axis',(1.,0.,0.));
#5268=DIRECTION('',(0.,0.,-1.));
#5269=DIRECTION('center_axis',(0.,0.,1.));
#5270=DIRECTION('ref_axis',(1.,0.,0.));
#5271=DIRECTION('center_axis',(0.,0.,1.));
#5272=DIRECTION('ref_axis',(1.,0.,0.));
#5273=DIRECTION('center_axis',(0.,0.,1.));
#5274=DIRECTION('ref_axis',(1.,0.,0.));
#5275=DIRECTION('axis',(0.,0.,1.));
#5276=DIRECTION('refdir',(1.,0.,0.));
#5277=DIRECTION('center_axis',(0.,1.,0.));
#5278=DIRECTION('ref_axis',(1.,0.,0.));
#5279=DIRECTION('center_axis',(0.,-1.,0.));
#5280=DIRECTION('ref_axis',(1.,0.,0.));
#5281=DIRECTION('',(0.,-1.,0.));
#5282=DIRECTION('center_axis',(0.,-1.,0.));
#5283=DIRECTION('ref_axis',(1.,0.,0.));
#5284=DIRECTION('center_axis',(0.,1.,0.));
#5285=DIRECTION('ref_axis',(1.,0.,0.));
#5286=DIRECTION('center_axis',(0.,1.,0.));
#5287=DIRECTION('ref_axis',(1.,0.,0.));
#5288=DIRECTION('',(0.,-1.,0.));
#5289=DIRECTION('center_axis',(0.,1.,0.));
#5290=DIRECTION('ref_axis',(1.,0.,0.));
#5291=DIRECTION('center_axis',(0.,1.,0.));
#5292=DIRECTION('ref_axis',(1.,0.,0.));
#5293=DIRECTION('center_axis',(0.,1.,0.));
#5294=DIRECTION('ref_axis',(1.,0.,0.));
#5295=DIRECTION('axis',(0.,0.,1.));
#5296=DIRECTION('refdir',(1.,0.,0.));
#5297=DIRECTION('center_axis',(0.,1.,0.));
#5298=DIRECTION('ref_axis',(0.,0.,1.));
#5299=DIRECTION('center_axis',(0.,-1.,0.));
#5300=DIRECTION('ref_axis',(1.,0.,0.));
#5301=DIRECTION('center_axis',(0.,-1.,0.));
#5302=DIRECTION('ref_axis',(1.,0.,0.));
#5303=DIRECTION('center_axis',(0.,-1.,0.));
#5304=DIRECTION('ref_axis',(1.,0.,0.));
#5305=DIRECTION('',(0.707106781186548,0.707106781186547,8.65956056235494E-17));
#5306=DIRECTION('center_axis',(0.,-1.,0.));
#5307=DIRECTION('ref_axis',(1.,0.,0.));
#5308=DIRECTION('center_axis',(0.,-1.,0.));
#5309=DIRECTION('ref_axis',(1.,0.,0.));
#5310=DIRECTION('',(0.,1.,0.));
#5311=DIRECTION('center_axis',(0.,1.,0.));
#5312=DIRECTION('ref_axis',(1.,0.,0.));
#5313=DIRECTION('center_axis',(0.,-1.,0.));
#5314=DIRECTION('ref_axis',(1.,0.,0.));
#5315=DIRECTION('',(-0.707106781186547,0.707106781186548,-8.65956056235493E-17));
#5316=DIRECTION('center_axis',(0.,-1.,0.));
#5317=DIRECTION('ref_axis',(0.,0.,-1.));
#5318=DIRECTION('center_axis',(0.,-1.,0.));
#5319=DIRECTION('ref_axis',(1.,0.,0.));
#5320=DIRECTION('center_axis',(0.,1.,0.));
#5321=DIRECTION('ref_axis',(1.,0.,0.));
#5322=DIRECTION('center_axis',(0.,1.,0.));
#5323=DIRECTION('ref_axis',(1.,0.,0.));
#5324=DIRECTION('',(-0.447213595499958,0.894427190999916,-5.47678698264203E-17));
#5325=DIRECTION('center_axis',(0.,-1.,0.));
#5326=DIRECTION('ref_axis',(1.,0.,0.));
#5327=DIRECTION('center_axis',(0.,1.,0.));
#5328=DIRECTION('ref_axis',(1.,0.,0.));
#5329=DIRECTION('',(0.,1.,0.));
#5330=DIRECTION('center_axis',(0.,1.,0.));
#5331=DIRECTION('ref_axis',(1.,0.,0.));
#5332=DIRECTION('center_axis',(0.,-1.,0.));
#5333=DIRECTION('ref_axis',(1.,0.,0.));
#5334=DIRECTION('',(-0.707106781186547,0.707106781186548,-8.65956056235493E-17));
#5335=DIRECTION('center_axis',(0.,-1.,0.));
#5336=DIRECTION('ref_axis',(0.,0.,-1.));
#5337=DIRECTION('center_axis',(0.866025403784439,0.,-0.5));
#5338=DIRECTION('ref_axis',(0.5,0.,0.866025403784439));
#5339=DIRECTION('',(-0.5,0.,-0.866025403784439));
#5340=DIRECTION('',(0.,-1.,0.));
#5341=DIRECTION('',(0.5,0.,0.866025403784439));
#5342=DIRECTION('',(0.,-1.,0.));
#5343=DIRECTION('center_axis',(1.92296268638356E-16,0.,-1.));
#5344=DIRECTION('ref_axis',(1.,0.,1.92296268638356E-16));
#5345=DIRECTION('',(-1.,0.,-1.92296268638356E-16));
#5346=DIRECTION('',(0.,-1.,0.));
#5347=DIRECTION('',(1.,0.,1.92296268638356E-16));
#5348=DIRECTION('center_axis',(-0.866025403784439,0.,-0.5));
#5349=DIRECTION('ref_axis',(0.5,0.,-0.866025403784439));
#5350=DIRECTION('',(-0.5,0.,0.866025403784438));
#5351=DIRECTION('',(0.,-1.,0.));
#5352=DIRECTION('',(0.5,0.,-0.866025403784438));
#5353=DIRECTION('center_axis',(-0.866025403784439,0.,0.5));
#5354=DIRECTION('ref_axis',(-0.5,0.,-0.866025403784439));
#5355=DIRECTION('',(0.5,0.,0.866025403784439));
#5356=DIRECTION('',(0.,-1.,0.));
#5357=DIRECTION('',(-0.5,0.,-0.866025403784439));
#5358=DIRECTION('center_axis',(-1.92296268638356E-16,0.,1.));
#5359=DIRECTION('ref_axis',(-1.,0.,-1.92296268638356E-16));
#5360=DIRECTION('',(1.,0.,1.92296268638356E-16));
#5361=DIRECTION('',(0.,-1.,0.));
#5362=DIRECTION('',(-1.,0.,-1.92296268638356E-16));
#5363=DIRECTION('center_axis',(0.866025403784439,0.,0.5));
#5364=DIRECTION('ref_axis',(-0.5,0.,0.866025403784439));
#5365=DIRECTION('',(0.5,0.,-0.866025403784439));
#5366=DIRECTION('',(-0.5,0.,0.866025403784439));
#5367=DIRECTION('center_axis',(0.,1.,0.));
#5368=DIRECTION('ref_axis',(1.,0.,0.));
#5369=DIRECTION('center_axis',(0.,-1.,0.));
#5370=DIRECTION('ref_axis',(0.,0.,-1.));
#5371=DIRECTION('',(0.,0.,1.));
#5372=DIRECTION('',(1.,0.,0.));
#5373=DIRECTION('',(0.,0.,1.));
#5374=DIRECTION('',(1.,0.,0.));
#5375=DIRECTION('',(0.,0.,1.));
#5376=DIRECTION('',(2.22044604925031E-16,-1.,0.));
#5377=DIRECTION('',(0.,0.,1.));
#5378=DIRECTION('',(2.22044604925031E-16,-1.,0.));
#5379=DIRECTION('',(0.,0.,1.));
#5380=DIRECTION('',(1.,0.,0.));
#5381=DIRECTION('',(0.,0.,1.));
#5382=DIRECTION('',(1.,0.,0.));
#5383=DIRECTION('',(0.,0.,1.));
#5384=DIRECTION('',(2.22044604925031E-16,1.,0.));
#5385=DIRECTION('',(0.,0.,1.));
#5386=DIRECTION('',(2.22044604925031E-16,1.,0.));
#5387=DIRECTION('',(0.,0.,1.));
#5388=DIRECTION('',(2.22044604925031E-16,1.,0.));
#5389=DIRECTION('',(0.,0.,1.));
#5390=DIRECTION('',(2.22044604925031E-16,1.,0.));
#5391=DIRECTION('',(0.,0.,1.));
#5392=DIRECTION('',(2.22044604925031E-16,-1.,0.));
#5393=DIRECTION('',(0.,0.,1.));
#5394=DIRECTION('',(2.22044604925031E-16,-1.,0.));
#5395=DIRECTION('',(0.,0.,1.));
#5396=DIRECTION('',(2.22044604925031E-16,-1.,0.));
#5397=DIRECTION('',(0.,0.,1.));
#5398=DIRECTION('',(2.22044604925031E-16,-1.,0.));
#5399=DIRECTION('',(0.,-1.,2.22044604925031E-16));
#5400=DIRECTION('',(1.,0.,0.));
#5401=DIRECTION('',(0.,-1.,2.22044604925031E-16));
#5402=DIRECTION('',(1.,0.,0.));
#5403=DIRECTION('',(0.,-1.,2.22044604925031E-16));
#5404=DIRECTION('',(1.,0.,0.));
#5405=DIRECTION('',(0.,-1.,2.22044604925031E-16));
#5406=DIRECTION('',(1.,0.,0.));
#5407=DIRECTION('',(0.,0.,1.));
#5408=DIRECTION('',(1.,0.,0.));
#5409=DIRECTION('',(0.,-1.,2.22044604925031E-16));
#5410=DIRECTION('',(1.,0.,0.));
#5411=DIRECTION('',(0.,-1.,2.22044604925031E-16));
#5412=DIRECTION('',(1.,0.,0.));
#5413=DIRECTION('',(0.,0.,1.));
#5414=DIRECTION('',(1.,0.,0.));
#5415=DIRECTION('',(0.,0.,1.));
#5416=DIRECTION('',(1.,0.,0.));
#5417=CARTESIAN_POINT('',(0.,0.,0.));
#5418=CARTESIAN_POINT('',(0.,0.,0.));
#5419=CARTESIAN_POINT('',(0.,0.,0.));
#5420=CARTESIAN_POINT('Origin',(26.5,-5.5,-0.1));
#5421=CARTESIAN_POINT('',(26.29,-5.5,0.));
#5422=CARTESIAN_POINT('Origin',(26.5,-5.5,0.));
#5423=CARTESIAN_POINT('',(26.29,-5.5,1.));
#5424=CARTESIAN_POINT('',(26.29,-5.5,-0.1));
#5425=CARTESIAN_POINT('Origin',(26.5,-5.5,1.));
#5426=CARTESIAN_POINT('Origin',(3.5,5.5,-0.1));
#5427=CARTESIAN_POINT('',(3.29,5.5,0.));
#5428=CARTESIAN_POINT('Origin',(3.5,5.5,0.));
#5429=CARTESIAN_POINT('',(3.29,5.5,1.));
#5430=CARTESIAN_POINT('',(3.29,5.5,-0.1));
#5431=CARTESIAN_POINT('Origin',(3.5,5.5,1.));
#5432=CARTESIAN_POINT('Origin',(3.5,-5.5,-0.1));
#5433=CARTESIAN_POINT('',(3.29,-5.5,0.));
#5434=CARTESIAN_POINT('Origin',(3.5,-5.5,0.));
#5435=CARTESIAN_POINT('',(3.29,-5.5,1.));
#5436=CARTESIAN_POINT('',(3.29,-5.5,-0.1));
#5437=CARTESIAN_POINT('Origin',(3.5,-5.5,1.));
#5438=CARTESIAN_POINT('Origin',(26.5,5.5,-0.1));
#5439=CARTESIAN_POINT('',(26.29,5.5,0.));
#5440=CARTESIAN_POINT('Origin',(26.5,5.5,0.));
#5441=CARTESIAN_POINT('',(26.29,5.5,1.));
#5442=CARTESIAN_POINT('',(26.29,5.5,-0.1));
#5443=CARTESIAN_POINT('Origin',(26.5,5.5,1.));
#5444=CARTESIAN_POINT('Origin',(29.,2.4,-0.1));
#5445=CARTESIAN_POINT('',(28.79,2.4,0.));
#5446=CARTESIAN_POINT('Origin',(29.,2.4,0.));
#5447=CARTESIAN_POINT('',(28.79,2.4,1.));
#5448=CARTESIAN_POINT('',(28.79,2.4,-0.1));
#5449=CARTESIAN_POINT('Origin',(29.,2.4,1.));
#5450=CARTESIAN_POINT('Origin',(29.,-5.6,-0.1));
#5451=CARTESIAN_POINT('',(28.79,-5.6,0.));
#5452=CARTESIAN_POINT('Origin',(29.,-5.6,0.));
#5453=CARTESIAN_POINT('',(28.79,-5.6,1.));
#5454=CARTESIAN_POINT('',(28.79,-5.6,-0.1));
#5455=CARTESIAN_POINT('Origin',(29.,-5.6,1.));
#5456=CARTESIAN_POINT('Origin',(1.,5.6,-0.1));
#5457=CARTESIAN_POINT('',(0.79,5.6,0.));
#5458=CARTESIAN_POINT('Origin',(1.,5.6,0.));
#5459=CARTESIAN_POINT('',(0.79,5.6,1.));
#5460=CARTESIAN_POINT('',(0.79,5.6,-0.1));
#5461=CARTESIAN_POINT('Origin',(1.,5.6,1.));
#5462=CARTESIAN_POINT('Origin',(1.,-2.4,-0.1));
#5463=CARTESIAN_POINT('',(0.79,-2.4,0.));
#5464=CARTESIAN_POINT('Origin',(1.,-2.4,0.));
#5465=CARTESIAN_POINT('',(0.79,-2.4,1.));
#5466=CARTESIAN_POINT('',(0.79,-2.4,-0.1));
#5467=CARTESIAN_POINT('Origin',(1.,-2.4,1.));
#5468=CARTESIAN_POINT('Origin',(1.,2.4,-0.1));
#5469=CARTESIAN_POINT('',(0.79,2.4,0.));
#5470=CARTESIAN_POINT('Origin',(1.,2.4,0.));
#5471=CARTESIAN_POINT('',(0.79,2.4,1.));
#5472=CARTESIAN_POINT('',(0.79,2.4,-0.1));
#5473=CARTESIAN_POINT('Origin',(1.,2.4,1.));
#5474=CARTESIAN_POINT('Origin',(1.,-5.6,-0.1));
#5475=CARTESIAN_POINT('',(0.79,-5.6,0.));
#5476=CARTESIAN_POINT('Origin',(1.,-5.6,0.));
#5477=CARTESIAN_POINT('',(0.79,-5.6,1.));
#5478=CARTESIAN_POINT('',(0.79,-5.6,-0.1));
#5479=CARTESIAN_POINT('Origin',(1.,-5.6,1.));
#5480=CARTESIAN_POINT('Origin',(29.,-2.4,-0.1));
#5481=CARTESIAN_POINT('',(28.79,-2.4,0.));
#5482=CARTESIAN_POINT('Origin',(29.,-2.4,0.));
#5483=CARTESIAN_POINT('',(28.79,-2.4,1.));
#5484=CARTESIAN_POINT('',(28.79,-2.4,-0.1));
#5485=CARTESIAN_POINT('Origin',(29.,-2.4,1.));
#5486=CARTESIAN_POINT('Origin',(29.,5.6,-0.1));
#5487=CARTESIAN_POINT('',(28.79,5.6,0.));
#5488=CARTESIAN_POINT('Origin',(29.,5.6,0.));
#5489=CARTESIAN_POINT('',(28.79,5.6,1.));
#5490=CARTESIAN_POINT('',(28.79,5.6,-0.1));
#5491=CARTESIAN_POINT('Origin',(29.,5.6,1.));
#5492=CARTESIAN_POINT('Origin',(31.,7.5,0.));
#5493=CARTESIAN_POINT('',(31.,7.5,0.));
#5494=CARTESIAN_POINT('',(-1.,7.5,0.));
#5495=CARTESIAN_POINT('',(31.,7.5,0.));
#5496=CARTESIAN_POINT('',(-1.,7.5,1.));
#5497=CARTESIAN_POINT('',(-1.,7.5,0.));
#5498=CARTESIAN_POINT('',(31.,7.5,1.));
#5499=CARTESIAN_POINT('',(31.,7.5,1.));
#5500=CARTESIAN_POINT('',(31.,7.5,0.));
#5501=CARTESIAN_POINT('Origin',(31.,-7.5,0.));
#5502=CARTESIAN_POINT('',(31.,-7.5,0.));
#5503=CARTESIAN_POINT('',(31.,-7.5,0.));
#5504=CARTESIAN_POINT('',(31.,-7.5,1.));
#5505=CARTESIAN_POINT('',(31.,-7.5,1.));
#5506=CARTESIAN_POINT('',(31.,-7.5,0.));
#5507=CARTESIAN_POINT('Origin',(-1.,-7.5,0.));
#5508=CARTESIAN_POINT('',(-1.,-7.5,0.));
#5509=CARTESIAN_POINT('',(-1.,-7.5,0.));
#5510=CARTESIAN_POINT('',(-1.,-7.5,1.));
#5511=CARTESIAN_POINT('',(-1.,-7.5,1.));
#5512=CARTESIAN_POINT('',(-1.,-7.5,0.));
#5513=CARTESIAN_POINT('Origin',(-1.,7.5,0.));
#5514=CARTESIAN_POINT('',(-1.,7.5,0.));
#5515=CARTESIAN_POINT('',(-1.,7.5,1.));
#5516=CARTESIAN_POINT('Origin',(15.,0.,1.));
#5517=CARTESIAN_POINT('Origin',(15.,0.,0.));
#5518=CARTESIAN_POINT('',(0.,0.,0.));
#5519=CARTESIAN_POINT('Origin',(0.05,0.,0.));
#5520=CARTESIAN_POINT('',(0.1,7.34788079488412E-17,0.6));
#5521=CARTESIAN_POINT('Origin',(0.1,0.,0.));
#5522=CARTESIAN_POINT('',(0.,-6.12323399573677E-17,0.5));
#5523=CARTESIAN_POINT('',(0.05,-6.73555739531044E-17,0.55));
#5524=CARTESIAN_POINT('Origin',(0.,0.,0.));
#5525=CARTESIAN_POINT('Origin',(0.,0.,0.));
#5526=CARTESIAN_POINT('',(29.9,-7.34788079488412E-17,0.6));
#5527=CARTESIAN_POINT('Origin',(29.9,0.,0.));
#5528=CARTESIAN_POINT('',(0.,-7.34788079488412E-17,0.6));
#5529=CARTESIAN_POINT('Origin',(0.,0.,0.));
#5530=CARTESIAN_POINT('Origin',(29.95,0.,0.));
#5531=CARTESIAN_POINT('',(30.,6.12323399573677E-17,0.5));
#5532=CARTESIAN_POINT('Origin',(30.,0.,0.));
#5533=CARTESIAN_POINT('',(29.95,-6.73555739531044E-17,0.55));
#5534=CARTESIAN_POINT('Origin',(30.,0.,0.));
#5535=CARTESIAN_POINT('',(0.,0.,0.));
#5536=CARTESIAN_POINT('Origin',(-1.6,0.,1.3));
#5537=CARTESIAN_POINT('',(-1.2,0.340036762718386,1.3));
#5538=CARTESIAN_POINT('',(-1.2,-0.340036762718386,1.3));
#5539=CARTESIAN_POINT('',(-1.2,0.,1.3));
#5540=CARTESIAN_POINT('Origin',(-1.6,0.,1.3));
#5541=CARTESIAN_POINT('Origin',(-1.6,0.,0.6));
#5542=CARTESIAN_POINT('',(-1.2,0.340036762718386,0.6));
#5543=CARTESIAN_POINT('',(-1.2,0.340036762718386,0.6));
#5544=CARTESIAN_POINT('',(-1.2,-0.340036762718386,0.6));
#5545=CARTESIAN_POINT('Origin',(-1.6,0.,0.6));
#5546=CARTESIAN_POINT('',(-1.2,-0.340036762718386,0.6));
#5547=CARTESIAN_POINT('Origin',(1.6,0.,0.6));
#5548=CARTESIAN_POINT('',(1.2,0.340036762718386,1.3));
#5549=CARTESIAN_POINT('',(1.2,0.340036762718386,0.6));
#5550=CARTESIAN_POINT('',(1.2,0.340036762718386,0.6));
#5551=CARTESIAN_POINT('',(1.2,-0.340036762718386,1.3));
#5552=CARTESIAN_POINT('Origin',(1.6,0.,1.3));
#5553=CARTESIAN_POINT('',(1.2,-0.340036762718386,0.6));
#5554=CARTESIAN_POINT('',(1.2,-0.340036762718386,0.6));
#5555=CARTESIAN_POINT('Origin',(1.6,0.,0.6));
#5556=CARTESIAN_POINT('Origin',(1.6,0.,1.3));
#5557=CARTESIAN_POINT('',(1.2,0.,1.3));
#5558=CARTESIAN_POINT('Origin',(-2.1,0.,0.6));
#5559=CARTESIAN_POINT('',(-1.2,0.7,0.6));
#5560=CARTESIAN_POINT('',(-1.2,0.,0.6));
#5561=CARTESIAN_POINT('',(-2.1,0.7,0.6));
#5562=CARTESIAN_POINT('',(-1.2,0.7,0.6));
#5563=CARTESIAN_POINT('',(-2.1,-0.7,0.6));
#5564=CARTESIAN_POINT('',(-2.1,0.,0.6));
#5565=CARTESIAN_POINT('',(-1.2,-0.7,0.6));
#5566=CARTESIAN_POINT('',(-1.2,-0.7,0.6));
#5567=CARTESIAN_POINT('',(-1.2,0.,0.6));
#5568=CARTESIAN_POINT('',(-1.875,3.36777869765522E-17,0.6));
#5569=CARTESIAN_POINT('Origin',(-1.6,0.,0.6));
#5570=CARTESIAN_POINT('Origin',(-1.2,0.,0.6));
#5571=CARTESIAN_POINT('',(-1.2,-0.7,3.75));
#5572=CARTESIAN_POINT('',(-1.2,-0.7,3.75));
#5573=CARTESIAN_POINT('',(-1.2,0.7,3.75));
#5574=CARTESIAN_POINT('',(-1.2,0.,3.75));
#5575=CARTESIAN_POINT('',(-1.2,0.7,3.75));
#5576=CARTESIAN_POINT('',(-1.2,-2.02066721859313E-17,3.515));
#5577=CARTESIAN_POINT('Origin',(-1.2,0.,3.35));
#5578=CARTESIAN_POINT('Origin',(1.2,0.,0.6));
#5579=CARTESIAN_POINT('',(2.1,-0.7,0.6));
#5580=CARTESIAN_POINT('',(2.1,0.7,0.6));
#5581=CARTESIAN_POINT('',(2.1,0.,0.6));
#5582=CARTESIAN_POINT('',(1.2,0.7,0.6));
#5583=CARTESIAN_POINT('',(2.1,0.7,0.6));
#5584=CARTESIAN_POINT('',(1.2,0.,0.6));
#5585=CARTESIAN_POINT('',(1.2,-0.7,0.6));
#5586=CARTESIAN_POINT('',(1.2,0.,0.6));
#5587=CARTESIAN_POINT('',(2.1,-0.7,0.6));
#5588=CARTESIAN_POINT('',(1.325,3.36777869765522E-17,0.6));
#5589=CARTESIAN_POINT('Origin',(1.6,0.,0.6));
#5590=CARTESIAN_POINT('Origin',(0.1,0.,3.35));
#5591=CARTESIAN_POINT('',(0.1,-2.75545529808155E-17,3.575));
#5592=CARTESIAN_POINT('Origin',(0.1,0.,3.35));
#5593=CARTESIAN_POINT('',(1.2,2.75545529808155E-17,3.575));
#5594=CARTESIAN_POINT('',(0.1,-2.75545529808155E-17,3.575));
#5595=CARTESIAN_POINT('Origin',(1.2,0.,3.35));
#5596=CARTESIAN_POINT('Origin',(0.,0.,3.35));
#5597=CARTESIAN_POINT('',(-0.1,2.02066721859313E-17,3.515));
#5598=CARTESIAN_POINT('',(0.,-2.02066721859313E-17,3.515));
#5599=CARTESIAN_POINT('Origin',(-0.1,0.,3.35));
#5600=CARTESIAN_POINT('Origin',(-1.6,0.,-0.05));
#5601=CARTESIAN_POINT('',(-1.875,-3.36777869765522E-17,0.));
#5602=CARTESIAN_POINT('Origin',(-1.6,0.,0.));
#5603=CARTESIAN_POINT('',(-1.875,-3.36777869765522E-17,-0.05));
#5604=CARTESIAN_POINT('Origin',(1.6,0.,-0.05));
#5605=CARTESIAN_POINT('',(1.325,-3.36777869765522E-17,0.));
#5606=CARTESIAN_POINT('Origin',(1.6,0.,0.));
#5607=CARTESIAN_POINT('',(1.325,-3.36777869765522E-17,-0.05));
#5608=CARTESIAN_POINT('Origin',(0.,0.,2.3));
#5609=CARTESIAN_POINT('',(-0.6,-0.7,2.3));
#5610=CARTESIAN_POINT('Origin',(0.,-0.7,2.3));
#5611=CARTESIAN_POINT('',(-0.6,0.7,2.3));
#5612=CARTESIAN_POINT('',(-0.6,0.,2.3));
#5613=CARTESIAN_POINT('Origin',(0.,0.7,2.3));
#5614=CARTESIAN_POINT('Origin',(0.,-0.7,1.875));
#5615=CARTESIAN_POINT('',(-2.1,-0.7,0.));
#5616=CARTESIAN_POINT('',(-2.1,-0.7,0.6));
#5617=CARTESIAN_POINT('',(2.1,-0.7,0.));
#5618=CARTESIAN_POINT('',(-2.1,-0.7,0.));
#5619=CARTESIAN_POINT('',(2.1,-0.7,0.));
#5620=CARTESIAN_POINT('',(1.2,-0.7,3.75));
#5621=CARTESIAN_POINT('',(1.2,-0.7,0.6));
#5622=CARTESIAN_POINT('',(0.1,-0.7,3.75));
#5623=CARTESIAN_POINT('',(1.2,-0.7,3.75));
#5624=CARTESIAN_POINT('',(0.1,-0.7,2.95));
#5625=CARTESIAN_POINT('',(0.1,-0.7,3.75));
#5626=CARTESIAN_POINT('',(-0.1,-0.7,2.95));
#5627=CARTESIAN_POINT('',(0.1,-0.7,2.95));
#5628=CARTESIAN_POINT('',(-0.1,-0.7,3.75));
#5629=CARTESIAN_POINT('',(-0.1,-0.7,2.95));
#5630=CARTESIAN_POINT('',(-0.1,-0.7,3.75));
#5631=CARTESIAN_POINT('Origin',(-2.1,0.,0.));
#5632=CARTESIAN_POINT('',(-2.1,0.7,0.));
#5633=CARTESIAN_POINT('',(-2.1,0.7,0.6));
#5634=CARTESIAN_POINT('',(-2.1,0.,0.));
#5635=CARTESIAN_POINT('Origin',(2.1,0.,0.));
#5636=CARTESIAN_POINT('',(2.1,0.7,0.));
#5637=CARTESIAN_POINT('',(-2.1,0.7,0.));
#5638=CARTESIAN_POINT('',(2.1,0.,0.));
#5639=CARTESIAN_POINT('Origin',(2.1,0.,0.6));
#5640=CARTESIAN_POINT('',(2.1,0.7,0.));
#5641=CARTESIAN_POINT('Origin',(1.2,0.,3.75));
#5642=CARTESIAN_POINT('',(1.2,0.7,3.75));
#5643=CARTESIAN_POINT('',(1.2,0.7,0.6));
#5644=CARTESIAN_POINT('',(1.2,0.,3.75));
#5645=CARTESIAN_POINT('Origin',(0.1,0.,3.75));
#5646=CARTESIAN_POINT('',(0.1,0.7,3.75));
#5647=CARTESIAN_POINT('',(1.2,0.7,3.75));
#5648=CARTESIAN_POINT('',(0.1,0.,3.75));
#5649=CARTESIAN_POINT('Origin',(0.1,0.,2.95));
#5650=CARTESIAN_POINT('',(0.1,0.7,2.95));
#5651=CARTESIAN_POINT('',(0.1,0.7,3.75));
#5652=CARTESIAN_POINT('',(0.1,0.,2.95));
#5653=CARTESIAN_POINT('Origin',(-0.1,0.,2.95));
#5654=CARTESIAN_POINT('',(-0.1,0.7,2.95));
#5655=CARTESIAN_POINT('',(0.1,0.7,2.95));
#5656=CARTESIAN_POINT('',(-0.1,0.,2.95));
#5657=CARTESIAN_POINT('Origin',(-0.1,0.,3.75));
#5658=CARTESIAN_POINT('',(-0.1,0.7,3.75));
#5659=CARTESIAN_POINT('',(-0.1,0.7,2.95));
#5660=CARTESIAN_POINT('',(-0.1,0.,3.75));
#5661=CARTESIAN_POINT('Origin',(-1.2,0.,3.75));
#5662=CARTESIAN_POINT('',(-0.1,0.7,3.75));
#5663=CARTESIAN_POINT('Origin',(0.,0.7,1.875));
#5664=CARTESIAN_POINT('',(0.,0.,0.));
#5665=CARTESIAN_POINT('Origin',(0.115470053837925,-0.5,-0.2));
#5666=CARTESIAN_POINT('',(0.23094010767585,-0.5,0.));
#5667=CARTESIAN_POINT('',(0.115470053837925,-0.5,-0.2));
#5668=CARTESIAN_POINT('',(0.23094010767585,-0.5,0.));
#5669=CARTESIAN_POINT('',(0.115470053837925,-0.8,-0.2));
#5670=CARTESIAN_POINT('',(0.115470053837925,-0.5,-0.2));
#5671=CARTESIAN_POINT('',(0.23094010767585,-0.8,0.));
#5672=CARTESIAN_POINT('',(0.23094010767585,-0.8,0.));
#5673=CARTESIAN_POINT('',(0.23094010767585,-0.5,0.));
#5674=CARTESIAN_POINT('Origin',(-0.115470053837925,-0.5,-0.2));
#5675=CARTESIAN_POINT('',(-0.115470053837925,-0.5,-0.2));
#5676=CARTESIAN_POINT('',(0.115470053837925,-0.5,-0.2));
#5677=CARTESIAN_POINT('',(-0.115470053837925,-0.8,-0.2));
#5678=CARTESIAN_POINT('',(-0.115470053837925,-0.5,-0.2));
#5679=CARTESIAN_POINT('',(0.115470053837925,-0.8,-0.2));
#5680=CARTESIAN_POINT('Origin',(-0.23094010767585,-0.5,-2.77555756156289E-17));
#5681=CARTESIAN_POINT('',(-0.23094010767585,-0.5,-2.82820063659975E-17));
#5682=CARTESIAN_POINT('',(-0.115470053837925,-0.5,-0.2));
#5683=CARTESIAN_POINT('',(-0.23094010767585,-0.8,-2.77555756156289E-17));
#5684=CARTESIAN_POINT('',(-0.23094010767585,-0.5,-2.82820063659975E-17));
#5685=CARTESIAN_POINT('',(-0.115470053837925,-0.8,-0.2));
#5686=CARTESIAN_POINT('Origin',(-0.115470053837925,-0.5,0.2));
#5687=CARTESIAN_POINT('',(-0.115470053837925,-0.5,0.2));
#5688=CARTESIAN_POINT('',(-0.23094010767585,-0.5,-2.82820063659975E-17));
#5689=CARTESIAN_POINT('',(-0.115470053837925,-0.8,0.2));
#5690=CARTESIAN_POINT('',(-0.115470053837925,-0.5,0.2));
#5691=CARTESIAN_POINT('',(-0.23094010767585,-0.8,-2.82820063659975E-17));
#5692=CARTESIAN_POINT('Origin',(0.115470053837925,-0.5,0.2));
#5693=CARTESIAN_POINT('',(0.115470053837925,-0.5,0.2));
#5694=CARTESIAN_POINT('',(-0.115470053837925,-0.5,0.2));
#5695=CARTESIAN_POINT('',(0.115470053837925,-0.8,0.2));
#5696=CARTESIAN_POINT('',(0.115470053837925,-0.5,0.2));
#5697=CARTESIAN_POINT('',(-0.115470053837925,-0.8,0.2));
#5698=CARTESIAN_POINT('Origin',(0.23094010767585,-0.5,0.));
#5699=CARTESIAN_POINT('',(0.115470053837925,-0.5,0.2));
#5700=CARTESIAN_POINT('',(0.115470053837925,-0.8,0.2));
#5701=CARTESIAN_POINT('Origin',(0.,-0.5,0.));
#5702=CARTESIAN_POINT('Origin',(0.,-0.8,0.));
#5703=CARTESIAN_POINT('Origin',(0.,-1.4,0.));
#5704=CARTESIAN_POINT('',(-0.24505,-1.4,3.00099698131059E-17));
#5705=CARTESIAN_POINT('Origin',(0.,-1.4,0.));
#5706=CARTESIAN_POINT('Origin',(0.375,0.5,0.));
#5707=CARTESIAN_POINT('',(-0.375,0.5,-4.59242549680257E-17));
#5708=CARTESIAN_POINT('Origin',(0.,0.5,0.));
#5709=CARTESIAN_POINT('Origin',(0.,0.475,0.));
#5710=CARTESIAN_POINT('',(-0.425,0.45,-5.20474889637625E-17));
#5711=CARTESIAN_POINT('Origin',(0.,0.45,0.));
#5712=CARTESIAN_POINT('',(-0.4,0.475,-4.89858719658941E-17));
#5713=CARTESIAN_POINT('Origin',(0.,0.24,0.));
#5714=CARTESIAN_POINT('',(-0.425,0.0299999999999998,-5.20474889637625E-17));
#5715=CARTESIAN_POINT('Origin',(0.,0.0299999999999998,0.));
#5716=CARTESIAN_POINT('',(-0.425,0.24,-5.20474889637625E-17));
#5717=CARTESIAN_POINT('Origin',(0.,0.0150000000000001,0.));
#5718=CARTESIAN_POINT('',(-0.395,4.85722573273506E-17,-4.83735485663204E-17));
#5719=CARTESIAN_POINT('Origin',(0.,0.,0.));
#5720=CARTESIAN_POINT('',(-0.41,0.0150000000000001,-5.02105187650415E-17));
#5721=CARTESIAN_POINT('Origin',(0.27,0.,0.));
#5722=CARTESIAN_POINT('',(-0.27,0.,-3.30654635769785E-17));
#5723=CARTESIAN_POINT('Origin',(0.,0.,0.));
#5724=CARTESIAN_POINT('Origin',(0.,-0.02,0.));
#5725=CARTESIAN_POINT('',(-0.24505,-0.0498999999999999,3.00099698131059E-17));
#5726=CARTESIAN_POINT('Origin',(0.,-0.0498999999999999,0.));
#5727=CARTESIAN_POINT('',(-0.26,-0.02,-3.18408167778312E-17));
#5728=CARTESIAN_POINT('Origin',(0.,-0.995,0.));
#5729=CARTESIAN_POINT('',(-0.24505,-0.995,-3.00099698131059E-17));
#5730=CARTESIAN_POINT('',(0.,0.,0.));
#5731=CARTESIAN_POINT('Origin',(3.5,-5.5,2.));
#5732=CARTESIAN_POINT('',(3.025,-5.5,2.));
#5733=CARTESIAN_POINT('Origin',(3.5,-5.5,2.));
#5734=CARTESIAN_POINT('',(3.025,-5.5,2.5));
#5735=CARTESIAN_POINT('',(3.025,-5.5,2.));
#5736=CARTESIAN_POINT('Origin',(3.5,-5.5,2.5));
#5737=CARTESIAN_POINT('Origin',(3.5,-5.5,2.));
#5738=CARTESIAN_POINT('',(3.225,-5.5,2.));
#5739=CARTESIAN_POINT('Origin',(3.5,-5.5,2.));
#5740=CARTESIAN_POINT('Origin',(3.5,5.5,2.));
#5741=CARTESIAN_POINT('',(3.025,5.5,2.));
#5742=CARTESIAN_POINT('Origin',(3.5,5.5,2.));
#5743=CARTESIAN_POINT('',(3.025,5.5,2.5));
#5744=CARTESIAN_POINT('',(3.025,5.5,2.));
#5745=CARTESIAN_POINT('Origin',(3.5,5.5,2.5));
#5746=CARTESIAN_POINT('Origin',(3.5,5.5,2.));
#5747=CARTESIAN_POINT('',(3.225,5.5,2.));
#5748=CARTESIAN_POINT('Origin',(3.5,5.5,2.));
#5749=CARTESIAN_POINT('Origin',(3.5,-5.5,0.9));
#5750=CARTESIAN_POINT('',(3.225,-5.5,1.));
#5751=CARTESIAN_POINT('Origin',(3.5,-5.5,1.));
#5752=CARTESIAN_POINT('',(3.225,-5.5,0.9));
#5753=CARTESIAN_POINT('Origin',(3.5,5.5,0.9));
#5754=CARTESIAN_POINT('',(3.225,5.5,1.));
#5755=CARTESIAN_POINT('Origin',(3.5,5.5,1.));
#5756=CARTESIAN_POINT('',(3.225,5.5,0.9));
#5757=CARTESIAN_POINT('Origin',(4.,6.5,1.));
#5758=CARTESIAN_POINT('',(4.,6.5,1.));
#5759=CARTESIAN_POINT('',(3.,6.5,1.));
#5760=CARTESIAN_POINT('',(4.,6.5,1.));
#5761=CARTESIAN_POINT('',(3.,6.5,2.5));
#5762=CARTESIAN_POINT('',(3.,6.5,1.));
#5763=CARTESIAN_POINT('',(4.,6.5,2.5));
#5764=CARTESIAN_POINT('',(4.,6.5,2.5));
#5765=CARTESIAN_POINT('',(4.,6.5,1.));
#5766=CARTESIAN_POINT('Origin',(4.,-6.5,1.));
#5767=CARTESIAN_POINT('',(4.,-6.5,1.));
#5768=CARTESIAN_POINT('',(4.,-6.5,1.));
#5769=CARTESIAN_POINT('',(4.,-6.5,2.5));
#5770=CARTESIAN_POINT('',(4.,-6.5,2.5));
#5771=CARTESIAN_POINT('',(4.,-6.5,1.));
#5772=CARTESIAN_POINT('Origin',(3.,-6.5,1.));
#5773=CARTESIAN_POINT('',(3.,-6.5,1.));
#5774=CARTESIAN_POINT('',(3.,-6.5,1.));
#5775=CARTESIAN_POINT('',(3.,-6.5,2.5));
#5776=CARTESIAN_POINT('',(3.,-6.5,2.5));
#5777=CARTESIAN_POINT('',(3.,-6.5,1.));
#5778=CARTESIAN_POINT('Origin',(3.,6.5,1.));
#5779=CARTESIAN_POINT('',(3.,6.5,1.));
#5780=CARTESIAN_POINT('',(3.,6.5,2.5));
#5781=CARTESIAN_POINT('Origin',(3.5,0.,2.5));
#5782=CARTESIAN_POINT('Origin',(3.5,0.,1.));
#5783=CARTESIAN_POINT('',(0.,0.,0.));
#5784=CARTESIAN_POINT('Origin',(4.2,6.,1.6));
#5785=CARTESIAN_POINT('',(4.2,6.,1.6));
#5786=CARTESIAN_POINT('',(4.,6.,1.6));
#5787=CARTESIAN_POINT('',(4.2,6.,1.6));
#5788=CARTESIAN_POINT('',(4.,6.,2.5));
#5789=CARTESIAN_POINT('',(4.,6.,1.6));
#5790=CARTESIAN_POINT('',(4.2,6.,2.5));
#5791=CARTESIAN_POINT('',(4.2,6.,2.5));
#5792=CARTESIAN_POINT('',(4.2,6.,1.6));
#5793=CARTESIAN_POINT('Origin',(4.2,-6.,1.6));
#5794=CARTESIAN_POINT('',(4.2,-6.,1.6));
#5795=CARTESIAN_POINT('',(4.2,-6.,1.6));
#5796=CARTESIAN_POINT('',(4.2,-6.,2.5));
#5797=CARTESIAN_POINT('',(4.2,-6.,2.5));
#5798=CARTESIAN_POINT('',(4.2,-6.,1.6));
#5799=CARTESIAN_POINT('Origin',(4.,-6.,1.6));
#5800=CARTESIAN_POINT('',(4.,-6.,1.6));
#5801=CARTESIAN_POINT('',(4.,-6.,1.6));
#5802=CARTESIAN_POINT('',(4.,-6.,2.5));
#5803=CARTESIAN_POINT('',(4.,-6.,2.5));
#5804=CARTESIAN_POINT('',(4.,-6.,1.6));
#5805=CARTESIAN_POINT('Origin',(4.,6.,1.6));
#5806=CARTESIAN_POINT('',(4.,6.,1.6));
#5807=CARTESIAN_POINT('',(4.,6.,2.5));
#5808=CARTESIAN_POINT('Origin',(4.1,0.,2.5));
#5809=CARTESIAN_POINT('Origin',(4.1,0.,1.6));
#5810=CARTESIAN_POINT('',(0.,0.,0.));
#5811=CARTESIAN_POINT('',(0.,0.,0.));
#5812=CARTESIAN_POINT('Origin',(13.4,5.5,3.));
#5813=CARTESIAN_POINT('',(13.5,5.5,3.165));
#5814=CARTESIAN_POINT('Origin',(13.5,5.5,3.));
#5815=CARTESIAN_POINT('',(16.5,5.5,3.165));
#5816=CARTESIAN_POINT('',(13.4,5.5,3.165));
#5817=CARTESIAN_POINT('Origin',(16.5,5.5,3.));
#5818=CARTESIAN_POINT('Origin',(13.4,-5.5,5.));
#5819=CARTESIAN_POINT('',(13.5,-5.5,5.165));
#5820=CARTESIAN_POINT('Origin',(13.5,-5.5,5.));
#5821=CARTESIAN_POINT('',(16.5,-5.5,5.165));
#5822=CARTESIAN_POINT('',(13.4,-5.5,5.165));
#5823=CARTESIAN_POINT('Origin',(16.5,-5.5,5.));
#5824=CARTESIAN_POINT('Origin',(13.4,-5.5,3.));
#5825=CARTESIAN_POINT('',(13.5,-5.5,3.165));
#5826=CARTESIAN_POINT('Origin',(13.5,-5.5,3.));
#5827=CARTESIAN_POINT('',(16.5,-5.5,3.165));
#5828=CARTESIAN_POINT('',(13.4,-5.5,3.165));
#5829=CARTESIAN_POINT('Origin',(16.5,-5.5,3.));
#5830=CARTESIAN_POINT('Origin',(13.4,5.5,5.));
#5831=CARTESIAN_POINT('',(13.5,5.5,5.165));
#5832=CARTESIAN_POINT('Origin',(13.5,5.5,5.));
#5833=CARTESIAN_POINT('',(16.5,5.5,5.165));
#5834=CARTESIAN_POINT('',(13.4,5.5,5.165));
#5835=CARTESIAN_POINT('Origin',(16.5,5.5,5.));
#5836=CARTESIAN_POINT('Origin',(16.,-2.2,4.4));
#5837=CARTESIAN_POINT('',(15.79,-2.2,4.4));
#5838=CARTESIAN_POINT('Origin',(16.,-2.2,4.4));
#5839=CARTESIAN_POINT('',(15.79,-2.2,5.8));
#5840=CARTESIAN_POINT('',(15.79,-2.2,4.4));
#5841=CARTESIAN_POINT('Origin',(16.,-2.2,5.8));
#5842=CARTESIAN_POINT('Origin',(16.,-2.2,4.4));
#5843=CARTESIAN_POINT('Origin',(14.,2.2,4.4));
#5844=CARTESIAN_POINT('',(13.79,2.2,4.4));
#5845=CARTESIAN_POINT('Origin',(14.,2.2,4.4));
#5846=CARTESIAN_POINT('',(13.79,2.2,5.8));
#5847=CARTESIAN_POINT('',(13.79,2.2,4.4));
#5848=CARTESIAN_POINT('Origin',(14.,2.2,5.8));
#5849=CARTESIAN_POINT('Origin',(14.,2.2,4.4));
#5850=CARTESIAN_POINT('Origin',(14.,-2.2,4.4));
#5851=CARTESIAN_POINT('',(13.79,-2.2,4.4));
#5852=CARTESIAN_POINT('Origin',(14.,-2.2,4.4));
#5853=CARTESIAN_POINT('',(13.79,-2.2,5.8));
#5854=CARTESIAN_POINT('',(13.79,-2.2,4.4));
#5855=CARTESIAN_POINT('Origin',(14.,-2.2,5.8));
#5856=CARTESIAN_POINT('Origin',(14.,-2.2,4.4));
#5857=CARTESIAN_POINT('Origin',(16.,2.2,4.4));
#5858=CARTESIAN_POINT('',(15.79,2.2,4.4));
#5859=CARTESIAN_POINT('Origin',(16.,2.2,4.4));
#5860=CARTESIAN_POINT('',(15.79,2.2,5.8));
#5861=CARTESIAN_POINT('',(15.79,2.2,4.4));
#5862=CARTESIAN_POINT('Origin',(16.,2.2,5.8));
#5863=CARTESIAN_POINT('Origin',(16.,2.2,4.4));
#5864=CARTESIAN_POINT('Origin',(13.4,-4.,3.3));
#5865=CARTESIAN_POINT('',(13.5,-4.,4.35));
#5866=CARTESIAN_POINT('Origin',(13.5,-4.,3.3));
#5867=CARTESIAN_POINT('',(16.5,-4.,4.35));
#5868=CARTESIAN_POINT('',(13.4,-4.,4.35));
#5869=CARTESIAN_POINT('Origin',(16.5,-4.,3.3));
#5870=CARTESIAN_POINT('Origin',(13.4,4.,3.3));
#5871=CARTESIAN_POINT('',(13.5,4.,4.35));
#5872=CARTESIAN_POINT('Origin',(13.5,4.,3.3));
#5873=CARTESIAN_POINT('',(16.5,4.,4.35));
#5874=CARTESIAN_POINT('',(13.4,4.,4.35));
#5875=CARTESIAN_POINT('Origin',(16.5,4.,3.3));
#5876=CARTESIAN_POINT('Origin',(16.5,6.,1.6));
#5877=CARTESIAN_POINT('',(16.5,6.,1.6));
#5878=CARTESIAN_POINT('',(13.5,6.,1.6));
#5879=CARTESIAN_POINT('',(16.5,6.,1.6));
#5880=CARTESIAN_POINT('',(13.5,6.,5.8));
#5881=CARTESIAN_POINT('',(13.5,6.,1.6));
#5882=CARTESIAN_POINT('',(16.5,6.,5.8));
#5883=CARTESIAN_POINT('',(16.5,6.,5.8));
#5884=CARTESIAN_POINT('',(16.5,6.,1.6));
#5885=CARTESIAN_POINT('Origin',(16.5,-6.,1.6));
#5886=CARTESIAN_POINT('',(16.5,-6.,1.6));
#5887=CARTESIAN_POINT('',(16.5,-6.,1.6));
#5888=CARTESIAN_POINT('',(16.5,-6.,5.8));
#5889=CARTESIAN_POINT('',(16.5,-6.,5.8));
#5890=CARTESIAN_POINT('',(16.5,-6.,1.6));
#5891=CARTESIAN_POINT('Origin',(13.5,-6.,1.6));
#5892=CARTESIAN_POINT('',(13.5,-6.,1.6));
#5893=CARTESIAN_POINT('',(13.5,-6.,1.6));
#5894=CARTESIAN_POINT('',(13.5,-6.,5.8));
#5895=CARTESIAN_POINT('',(13.5,-6.,5.8));
#5896=CARTESIAN_POINT('',(13.5,-6.,1.6));
#5897=CARTESIAN_POINT('Origin',(13.5,6.,1.6));
#5898=CARTESIAN_POINT('',(13.5,6.,1.6));
#5899=CARTESIAN_POINT('',(13.5,6.,5.8));
#5900=CARTESIAN_POINT('Origin',(15.,0.,5.8));
#5901=CARTESIAN_POINT('Origin',(15.,0.,1.6));
#5902=CARTESIAN_POINT('',(0.,0.,0.));
#5903=CARTESIAN_POINT('Origin',(15.,0.,5.7));
#5904=CARTESIAN_POINT('',(14.75,-3.06161699786838E-17,5.8));
#5905=CARTESIAN_POINT('Origin',(15.,0.,5.8));
#5906=CARTESIAN_POINT('',(14.75,3.06161699786838E-17,6.6));
#5907=CARTESIAN_POINT('',(14.75,-3.06161699786838E-17,5.7));
#5908=CARTESIAN_POINT('Origin',(15.,0.,6.6));
#5909=CARTESIAN_POINT('Origin',(16.,-2.2,5.7));
#5910=CARTESIAN_POINT('',(15.725,-2.2,5.8));
#5911=CARTESIAN_POINT('Origin',(16.,-2.2,5.8));
#5912=CARTESIAN_POINT('',(15.725,-2.2,6.6));
#5913=CARTESIAN_POINT('',(15.725,-2.2,5.7));
#5914=CARTESIAN_POINT('Origin',(16.,-2.2,6.6));
#5915=CARTESIAN_POINT('Origin',(14.,2.2,5.7));
#5916=CARTESIAN_POINT('',(13.725,2.2,5.8));
#5917=CARTESIAN_POINT('Origin',(14.,2.2,5.8));
#5918=CARTESIAN_POINT('',(13.725,2.2,6.6));
#5919=CARTESIAN_POINT('',(13.725,2.2,5.7));
#5920=CARTESIAN_POINT('Origin',(14.,2.2,6.6));
#5921=CARTESIAN_POINT('Origin',(14.,-2.2,5.7));
#5922=CARTESIAN_POINT('',(13.725,-2.2,5.8));
#5923=CARTESIAN_POINT('Origin',(14.,-2.2,5.8));
#5924=CARTESIAN_POINT('',(13.725,-2.2,6.6));
#5925=CARTESIAN_POINT('',(13.725,-2.2,5.7));
#5926=CARTESIAN_POINT('Origin',(14.,-2.2,6.6));
#5927=CARTESIAN_POINT('Origin',(16.,2.2,5.7));
#5928=CARTESIAN_POINT('',(15.725,2.2,5.8));
#5929=CARTESIAN_POINT('Origin',(16.,2.2,5.8));
#5930=CARTESIAN_POINT('',(15.725,2.2,6.6));
#5931=CARTESIAN_POINT('',(15.725,2.2,5.7));
#5932=CARTESIAN_POINT('Origin',(16.,2.2,6.6));
#5933=CARTESIAN_POINT('Origin',(18.,6.5,5.8));
#5934=CARTESIAN_POINT('',(18.,6.5,5.8));
#5935=CARTESIAN_POINT('',(12.,6.5,5.8));
#5936=CARTESIAN_POINT('',(18.,6.5,5.8));
#5937=CARTESIAN_POINT('',(12.,6.5,6.6));
#5938=CARTESIAN_POINT('',(12.,6.5,5.8));
#5939=CARTESIAN_POINT('',(18.,6.5,6.6));
#5940=CARTESIAN_POINT('',(18.,6.5,6.6));
#5941=CARTESIAN_POINT('',(18.,6.5,5.8));
#5942=CARTESIAN_POINT('Origin',(18.,-6.5,5.8));
#5943=CARTESIAN_POINT('',(18.,-6.5,5.8));
#5944=CARTESIAN_POINT('',(18.,-6.5,5.8));
#5945=CARTESIAN_POINT('',(18.,-6.5,6.6));
#5946=CARTESIAN_POINT('',(18.,-6.5,6.6));
#5947=CARTESIAN_POINT('',(18.,-6.5,5.8));
#5948=CARTESIAN_POINT('Origin',(12.,-6.5,5.8));
#5949=CARTESIAN_POINT('',(12.,-6.5,5.8));
#5950=CARTESIAN_POINT('',(12.,-6.5,5.8));
#5951=CARTESIAN_POINT('',(12.,-6.5,6.6));
#5952=CARTESIAN_POINT('',(12.,-6.5,6.6));
#5953=CARTESIAN_POINT('',(12.,-6.5,5.8));
#5954=CARTESIAN_POINT('Origin',(12.,6.5,5.8));
#5955=CARTESIAN_POINT('',(12.,6.5,5.8));
#5956=CARTESIAN_POINT('',(12.,6.5,6.6));
#5957=CARTESIAN_POINT('Origin',(15.,0.,6.6));
#5958=CARTESIAN_POINT('Origin',(15.,0.,5.8));
#5959=CARTESIAN_POINT('',(0.,0.,0.));
#5960=CARTESIAN_POINT('',(0.,0.,0.));
#5961=CARTESIAN_POINT('Origin',(0.75,1.2,0.));
#5962=CARTESIAN_POINT('',(0.885663593019381,1.2,-0.16));
#5963=CARTESIAN_POINT('',(0.885663593019381,1.2,0.16));
#5964=CARTESIAN_POINT('Origin',(0.,1.2,0.));
#5965=CARTESIAN_POINT('',(0.93,1.2,-0.16));
#5966=CARTESIAN_POINT('',(0.93,1.2,-0.16));
#5967=CARTESIAN_POINT('',(0.93,1.2,0.16));
#5968=CARTESIAN_POINT('',(0.93,1.2,0.16));
#5969=CARTESIAN_POINT('',(0.57,1.2,0.16));
#5970=CARTESIAN_POINT('Origin',(0.57,0.,0.16));
#5971=CARTESIAN_POINT('',(0.885663593019381,-1.2,0.16));
#5972=CARTESIAN_POINT('',(0.885663593019381,0.,0.16));
#5973=CARTESIAN_POINT('',(0.93,-1.2,0.16));
#5974=CARTESIAN_POINT('',(0.93,0.,0.16));
#5975=CARTESIAN_POINT('',(0.57,-1.2,0.16));
#5976=CARTESIAN_POINT('Origin',(0.75,-1.2,0.));
#5977=CARTESIAN_POINT('',(0.885663593019381,-1.2,-0.16));
#5978=CARTESIAN_POINT('Origin',(0.,-1.2,0.));
#5979=CARTESIAN_POINT('',(0.93,-1.2,-0.16));
#5980=CARTESIAN_POINT('',(0.93,-1.2,0.16));
#5981=CARTESIAN_POINT('',(0.93,-1.2,-0.16));
#5982=CARTESIAN_POINT('Origin',(0.93,0.,-0.16));
#5983=CARTESIAN_POINT('',(0.885663593019381,0.,-0.16));
#5984=CARTESIAN_POINT('',(0.93,0.,-0.16));
#5985=CARTESIAN_POINT('Origin',(0.93,0.,0.16));
#5986=CARTESIAN_POINT('Origin',(1.05,1.5,0.));
#5987=CARTESIAN_POINT('',(-1.05,1.5,-1.28587913910472E-16));
#5988=CARTESIAN_POINT('Origin',(0.,1.5,0.));
#5989=CARTESIAN_POINT('',(-0.9,1.5,-1.10218211923262E-16));
#5990=CARTESIAN_POINT('Origin',(0.,1.5,0.));
#5991=CARTESIAN_POINT('Origin',(0.,1.315,0.));
#5992=CARTESIAN_POINT('',(-1.05,1.13,-1.28587913910472E-16));
#5993=CARTESIAN_POINT('Origin',(0.,1.13,0.));
#5994=CARTESIAN_POINT('',(-1.05,1.315,-1.28587913910472E-16));
#5995=CARTESIAN_POINT('Origin',(1.,1.13,0.));
#5996=CARTESIAN_POINT('',(-1.,1.13,-1.22464679914735E-16));
#5997=CARTESIAN_POINT('Origin',(0.,1.13,0.));
#5998=CARTESIAN_POINT('Origin',(0.,1.065,0.));
#5999=CARTESIAN_POINT('',(-1.,1.,-1.22464679914735E-16));
#6000=CARTESIAN_POINT('Origin',(0.,1.,0.));
#6001=CARTESIAN_POINT('',(-1.,1.065,-1.22464679914735E-16));
#6002=CARTESIAN_POINT('Origin',(1.05,1.,0.));
#6003=CARTESIAN_POINT('',(-1.05,1.,-1.28587913910472E-16));
#6004=CARTESIAN_POINT('Origin',(0.,1.,0.));
#6005=CARTESIAN_POINT('Origin',(0.,0.,0.));
#6006=CARTESIAN_POINT('',(-1.05,-1.,-1.28587913910472E-16));
#6007=CARTESIAN_POINT('Origin',(0.,-1.,0.));
#6008=CARTESIAN_POINT('',(-1.05,0.,-1.28587913910472E-16));
#6009=CARTESIAN_POINT('Origin',(1.,-1.,0.));
#6010=CARTESIAN_POINT('',(-1.,-1.,-1.22464679914735E-16));
#6011=CARTESIAN_POINT('Origin',(0.,-1.,0.));
#6012=CARTESIAN_POINT('Origin',(0.,-1.065,0.));
#6013=CARTESIAN_POINT('',(-1.,-1.13,-1.22464679914735E-16));
#6014=CARTESIAN_POINT('Origin',(0.,-1.13,0.));
#6015=CARTESIAN_POINT('',(-1.,-1.065,-1.22464679914735E-16));
#6016=CARTESIAN_POINT('Origin',(1.05,-1.13,0.));
#6017=CARTESIAN_POINT('',(-1.05,-1.13,-1.28587913910472E-16));
#6018=CARTESIAN_POINT('Origin',(0.,-1.13,0.));
#6019=CARTESIAN_POINT('Origin',(0.,-1.315,0.));
#6020=CARTESIAN_POINT('',(-1.05,-1.5,-1.28587913910472E-16));
#6021=CARTESIAN_POINT('Origin',(0.,-1.5,0.));
#6022=CARTESIAN_POINT('',(-1.05,-1.315,-1.28587913910472E-16));
#6023=CARTESIAN_POINT('Origin',(0.9,-1.5,0.));
#6024=CARTESIAN_POINT('',(-0.9,-1.5,-1.10218211923262E-16));
#6025=CARTESIAN_POINT('Origin',(0.,-1.5,0.));
#6026=CARTESIAN_POINT('Origin',(0.,0.,0.));
#6027=CARTESIAN_POINT('',(-0.9,0.,-1.10218211923262E-16));
#6028=CARTESIAN_POINT('',(0.,0.,0.));
#6029=CARTESIAN_POINT('Origin',(0.75,1.2,0.));
#6030=CARTESIAN_POINT('',(0.880582193778639,1.2,0.16));
#6031=CARTESIAN_POINT('',(0.880582193778639,1.2,-0.16));
#6032=CARTESIAN_POINT('Origin',(0.,1.2,0.));
#6033=CARTESIAN_POINT('',(0.583459510163302,1.2,0.16));
#6034=CARTESIAN_POINT('',(0.57,1.2,0.16));
#6035=CARTESIAN_POINT('',(0.583459510163302,1.2,-0.16));
#6036=CARTESIAN_POINT('Origin',(0.,1.2,0.));
#6037=CARTESIAN_POINT('',(0.93,1.2,-0.16));
#6038=CARTESIAN_POINT('Origin',(0.93,0.,-0.16));
#6039=CARTESIAN_POINT('',(0.880582193778639,-1.2,-0.16));
#6040=CARTESIAN_POINT('',(0.880582193778639,0.,-0.16));
#6041=CARTESIAN_POINT('',(0.583459510163302,-1.2,-0.16));
#6042=CARTESIAN_POINT('',(0.583459510163302,0.,-0.16));
#6043=CARTESIAN_POINT('',(0.93,-1.2,-0.16));
#6044=CARTESIAN_POINT('Origin',(0.75,-1.2,0.));
#6045=CARTESIAN_POINT('',(0.880582193778639,-1.2,0.16));
#6046=CARTESIAN_POINT('Origin',(0.,-1.2,0.));
#6047=CARTESIAN_POINT('',(0.583459510163302,-1.2,0.16));
#6048=CARTESIAN_POINT('Origin',(0.,-1.2,0.));
#6049=CARTESIAN_POINT('',(0.57,-1.2,0.16));
#6050=CARTESIAN_POINT('Origin',(0.57,0.,0.16));
#6051=CARTESIAN_POINT('',(0.880582193778639,0.,0.16));
#6052=CARTESIAN_POINT('',(0.583459510163302,0.,0.16));
#6053=CARTESIAN_POINT('Origin',(0.895,1.35,0.));
#6054=CARTESIAN_POINT('',(-0.895,1.35,-1.09605888523688E-16));
#6055=CARTESIAN_POINT('Origin',(0.,1.35,0.));
#6056=CARTESIAN_POINT('',(-0.605,1.35,-7.40911313484149E-17));
#6057=CARTESIAN_POINT('Origin',(0.,1.35,0.));
#6058=CARTESIAN_POINT('Origin',(0.,0.,0.));
#6059=CARTESIAN_POINT('',(-0.895,-1.35,-1.09605888523688E-16));
#6060=CARTESIAN_POINT('Origin',(0.,-1.35,0.));
#6061=CARTESIAN_POINT('',(-0.895,0.,-1.09605888523688E-16));
#6062=CARTESIAN_POINT('Origin',(0.605,-1.35,0.));
#6063=CARTESIAN_POINT('',(-0.605,-1.35,-7.40911313484149E-17));
#6064=CARTESIAN_POINT('Origin',(0.,-1.35,0.));
#6065=CARTESIAN_POINT('Origin',(0.,0.,0.));
#6066=CARTESIAN_POINT('',(-0.605,0.,-7.40911313484149E-17));
#6067=CARTESIAN_POINT('',(0.,0.,0.));
#6068=CARTESIAN_POINT('',(0.,0.,0.));
#6069=CARTESIAN_POINT('',(0.,0.,0.));
#6070=CARTESIAN_POINT('Origin',(9.9,5.5,3.));
#6071=CARTESIAN_POINT('',(10.,5.5,3.225));
#6072=CARTESIAN_POINT('Origin',(10.,5.5,3.));
#6073=CARTESIAN_POINT('',(10.5,5.5,3.225));
#6074=CARTESIAN_POINT('',(9.9,5.5,3.225));
#6075=CARTESIAN_POINT('Origin',(10.5,5.5,3.));
#6076=CARTESIAN_POINT('Origin',(9.9,-5.5,5.));
#6077=CARTESIAN_POINT('',(10.,-5.5,5.225));
#6078=CARTESIAN_POINT('Origin',(10.,-5.5,5.));
#6079=CARTESIAN_POINT('',(10.5,-5.5,5.225));
#6080=CARTESIAN_POINT('',(9.9,-5.5,5.225));
#6081=CARTESIAN_POINT('Origin',(10.5,-5.5,5.));
#6082=CARTESIAN_POINT('Origin',(9.9,-5.5,3.));
#6083=CARTESIAN_POINT('',(10.,-5.5,3.225));
#6084=CARTESIAN_POINT('Origin',(10.,-5.5,3.));
#6085=CARTESIAN_POINT('',(10.5,-5.5,3.225));
#6086=CARTESIAN_POINT('',(9.9,-5.5,3.225));
#6087=CARTESIAN_POINT('Origin',(10.5,-5.5,3.));
#6088=CARTESIAN_POINT('Origin',(9.9,5.5,5.));
#6089=CARTESIAN_POINT('',(10.,5.5,5.225));
#6090=CARTESIAN_POINT('Origin',(10.,5.5,5.));
#6091=CARTESIAN_POINT('',(10.5,5.5,5.225));
#6092=CARTESIAN_POINT('',(9.9,5.5,5.225));
#6093=CARTESIAN_POINT('Origin',(10.5,5.5,5.));
#6094=CARTESIAN_POINT('Origin',(9.9,-4.,3.3));
#6095=CARTESIAN_POINT('',(10.,-4.,4.));
#6096=CARTESIAN_POINT('Origin',(10.,-4.,3.3));
#6097=CARTESIAN_POINT('',(10.5,-4.,4.));
#6098=CARTESIAN_POINT('',(9.9,-4.,4.));
#6099=CARTESIAN_POINT('Origin',(10.5,-4.,3.3));
#6100=CARTESIAN_POINT('Origin',(9.9,4.,3.3));
#6101=CARTESIAN_POINT('',(10.,4.,4.));
#6102=CARTESIAN_POINT('Origin',(10.,4.,3.3));
#6103=CARTESIAN_POINT('',(10.5,4.,4.));
#6104=CARTESIAN_POINT('',(9.9,4.,4.));
#6105=CARTESIAN_POINT('Origin',(10.5,4.,3.3));
#6106=CARTESIAN_POINT('Origin',(10.5,6.,1.6));
#6107=CARTESIAN_POINT('',(10.5,6.,1.6));
#6108=CARTESIAN_POINT('',(10.,6.,1.6));
#6109=CARTESIAN_POINT('',(10.5,6.,1.6));
#6110=CARTESIAN_POINT('',(10.,6.,5.8));
#6111=CARTESIAN_POINT('',(10.,6.,1.6));
#6112=CARTESIAN_POINT('',(10.5,6.,5.8));
#6113=CARTESIAN_POINT('',(10.5,6.,5.8));
#6114=CARTESIAN_POINT('',(10.5,6.,1.6));
#6115=CARTESIAN_POINT('Origin',(10.5,-6.,1.6));
#6116=CARTESIAN_POINT('',(10.5,-6.,1.6));
#6117=CARTESIAN_POINT('',(10.5,-6.,1.6));
#6118=CARTESIAN_POINT('',(10.5,-6.,5.8));
#6119=CARTESIAN_POINT('',(10.5,-6.,5.8));
#6120=CARTESIAN_POINT('',(10.5,-6.,1.6));
#6121=CARTESIAN_POINT('Origin',(10.,-6.,1.6));
#6122=CARTESIAN_POINT('',(10.,-6.,1.6));
#6123=CARTESIAN_POINT('',(10.,-6.,1.6));
#6124=CARTESIAN_POINT('',(10.,-6.,5.8));
#6125=CARTESIAN_POINT('',(10.,-6.,5.8));
#6126=CARTESIAN_POINT('',(10.,-6.,1.6));
#6127=CARTESIAN_POINT('Origin',(10.,6.,1.6));
#6128=CARTESIAN_POINT('',(10.,6.,1.6));
#6129=CARTESIAN_POINT('',(10.,6.,5.8));
#6130=CARTESIAN_POINT('Origin',(10.25,0.,5.8));
#6131=CARTESIAN_POINT('Origin',(10.25,0.,1.6));
#6132=CARTESIAN_POINT('',(0.,0.,0.));
#6133=CARTESIAN_POINT('Origin',(0.3,0.4,0.));
#6134=CARTESIAN_POINT('',(-0.3,0.4,-3.67394039744206E-17));
#6135=CARTESIAN_POINT('Origin',(0.,0.4,0.));
#6136=CARTESIAN_POINT('Origin',(0.,0.375,0.));
#6137=CARTESIAN_POINT('',(-0.35,0.35,-4.28626379701573E-17));
#6138=CARTESIAN_POINT('Origin',(0.,0.35,0.));
#6139=CARTESIAN_POINT('',(-0.325,0.375,-3.9801020972289E-17));
#6140=CARTESIAN_POINT('Origin',(0.,0.19,0.));
#6141=CARTESIAN_POINT('',(-0.35,0.03,-4.28626379701574E-17));
#6142=CARTESIAN_POINT('Origin',(0.,0.03,0.));
#6143=CARTESIAN_POINT('',(-0.35,0.19,-4.28626379701574E-17));
#6144=CARTESIAN_POINT('Origin',(0.,0.0149999999999999,0.));
#6145=CARTESIAN_POINT('',(-0.32,-3.29597460435593E-17,-3.91886975727153E-17));
#6146=CARTESIAN_POINT('Origin',(0.,0.,0.));
#6147=CARTESIAN_POINT('',(-0.335,0.0149999999999999,-4.10256677714363E-17));
#6148=CARTESIAN_POINT('Origin',(0.22,0.,0.));
#6149=CARTESIAN_POINT('',(-0.22,-6.93889390390723E-18,-2.69422295812418E-17));
#6150=CARTESIAN_POINT('Origin',(0.,0.,0.));
#6151=CARTESIAN_POINT('Origin',(0.,-0.02,0.));
#6152=CARTESIAN_POINT('',(-0.1954,-0.0492,2.39295984553393E-17));
#6153=CARTESIAN_POINT('Origin',(0.,-0.0492,0.));
#6154=CARTESIAN_POINT('',(-0.21,-0.02,-2.57175827820944E-17));
#6155=CARTESIAN_POINT('Origin',(0.,-0.8,0.));
#6156=CARTESIAN_POINT('',(-0.1954,-1.5646,2.39295984553393E-17));
#6157=CARTESIAN_POINT('Origin',(0.,-1.5646,0.));
#6158=CARTESIAN_POINT('',(-0.1954,-0.8,-2.39295984553393E-17));
#6159=CARTESIAN_POINT('Origin',(0.,-1.58,0.));
#6160=CARTESIAN_POINT('',(-0.16,-1.6,-1.95943487863577E-17));
#6161=CARTESIAN_POINT('Origin',(0.,-1.6,0.));
#6162=CARTESIAN_POINT('',(-0.18,-1.58,-2.20436423846524E-17));
#6163=CARTESIAN_POINT('Origin',(0.,-1.6,0.));
#6164=CARTESIAN_POINT('Origin',(0.0866025403784439,-0.4,-0.15));
#6165=CARTESIAN_POINT('',(0.173205080756888,-0.4,0.));
#6166=CARTESIAN_POINT('',(0.0866025403784439,-0.4,-0.15));
#6167=CARTESIAN_POINT('',(0.173205080756888,-0.4,0.));
#6168=CARTESIAN_POINT('',(0.0866025403784439,-0.64,-0.15));
#6169=CARTESIAN_POINT('',(0.0866025403784439,-0.4,-0.15));
#6170=CARTESIAN_POINT('',(0.173205080756888,-0.64,0.));
#6171=CARTESIAN_POINT('',(0.173205080756888,-0.64,0.));
#6172=CARTESIAN_POINT('',(0.173205080756888,-0.4,0.));
#6173=CARTESIAN_POINT('Origin',(-0.0866025403784438,-0.4,-0.15));
#6174=CARTESIAN_POINT('',(-0.0866025403784438,-0.4,-0.15));
#6175=CARTESIAN_POINT('',(0.0866025403784439,-0.4,-0.15));
#6176=CARTESIAN_POINT('',(-0.0866025403784438,-0.64,-0.15));
#6177=CARTESIAN_POINT('',(-0.0866025403784438,-0.4,-0.15));
#6178=CARTESIAN_POINT('',(0.0866025403784439,-0.64,-0.15));
#6179=CARTESIAN_POINT('Origin',(-0.173205080756888,-0.4,-2.77555756156289E-17));
#6180=CARTESIAN_POINT('',(-0.173205080756888,-0.4,-2.12115047744981E-17));
#6181=CARTESIAN_POINT('',(-0.0866025403784438,-0.4,-0.15));
#6182=CARTESIAN_POINT('',(-0.173205080756888,-0.64,-2.77555756156289E-17));
#6183=CARTESIAN_POINT('',(-0.173205080756888,-0.4,-2.12115047744981E-17));
#6184=CARTESIAN_POINT('',(-0.0866025403784438,-0.64,-0.15));
#6185=CARTESIAN_POINT('Origin',(-0.0866025403784439,-0.4,0.15));
#6186=CARTESIAN_POINT('',(-0.0866025403784439,-0.4,0.15));
#6187=CARTESIAN_POINT('',(-0.173205080756888,-0.4,-2.12115047744981E-17));
#6188=CARTESIAN_POINT('',(-0.0866025403784439,-0.64,0.15));
#6189=CARTESIAN_POINT('',(-0.0866025403784439,-0.4,0.15));
#6190=CARTESIAN_POINT('',(-0.173205080756888,-0.64,-2.12115047744981E-17));
#6191=CARTESIAN_POINT('Origin',(0.0866025403784439,-0.4,0.15));
#6192=CARTESIAN_POINT('',(0.0866025403784439,-0.4,0.15));
#6193=CARTESIAN_POINT('',(-0.0866025403784439,-0.4,0.15));
#6194=CARTESIAN_POINT('',(0.0866025403784439,-0.64,0.15));
#6195=CARTESIAN_POINT('',(0.0866025403784439,-0.4,0.15));
#6196=CARTESIAN_POINT('',(-0.0866025403784439,-0.64,0.15));
#6197=CARTESIAN_POINT('Origin',(0.173205080756888,-0.4,0.));
#6198=CARTESIAN_POINT('',(0.0866025403784439,-0.4,0.15));
#6199=CARTESIAN_POINT('',(0.0866025403784439,-0.64,0.15));
#6200=CARTESIAN_POINT('Origin',(0.,-0.4,-2.77555756156289E-17));
#6201=CARTESIAN_POINT('Origin',(0.,-0.64,-2.77555756156289E-17));
#6202=CARTESIAN_POINT('',(0.,0.,0.));
#6203=CARTESIAN_POINT('Origin',(0.375,0.5,0.));
#6204=CARTESIAN_POINT('',(-0.375,0.5,-4.59242549680257E-17));
#6205=CARTESIAN_POINT('Origin',(0.,0.5,0.));
#6206=CARTESIAN_POINT('Origin',(0.,0.475,0.));
#6207=CARTESIAN_POINT('',(-0.425,0.45,-5.20474889637625E-17));
#6208=CARTESIAN_POINT('Origin',(0.,0.45,0.));
#6209=CARTESIAN_POINT('',(-0.4,0.475,-4.89858719658941E-17));
#6210=CARTESIAN_POINT('Origin',(0.,0.24,0.));
#6211=CARTESIAN_POINT('',(-0.425,0.0299999999999998,-5.20474889637625E-17));
#6212=CARTESIAN_POINT('Origin',(0.,0.0299999999999998,0.));
#6213=CARTESIAN_POINT('',(-0.425,0.24,-5.20474889637625E-17));
#6214=CARTESIAN_POINT('Origin',(0.,0.0150000000000001,0.));
#6215=CARTESIAN_POINT('',(-0.395,4.85722573273506E-17,-4.83735485663204E-17));
#6216=CARTESIAN_POINT('Origin',(0.,0.,0.));
#6217=CARTESIAN_POINT('',(-0.41,0.0150000000000001,-5.02105187650415E-17));
#6218=CARTESIAN_POINT('Origin',(0.27,0.,0.));
#6219=CARTESIAN_POINT('',(-0.27,0.,-3.30654635769785E-17));
#6220=CARTESIAN_POINT('Origin',(0.,0.,0.));
#6221=CARTESIAN_POINT('Origin',(0.,-0.02,0.));
#6222=CARTESIAN_POINT('',(-0.24505,-0.0498999999999999,3.00099698131059E-17));
#6223=CARTESIAN_POINT('Origin',(0.,-0.0498999999999999,0.));
#6224=CARTESIAN_POINT('',(-0.26,-0.02,-3.18408167778312E-17));
#6225=CARTESIAN_POINT('Origin',(0.,-0.995,0.));
#6226=CARTESIAN_POINT('',(-0.24505,-1.95495,3.00099698131059E-17));
#6227=CARTESIAN_POINT('Origin',(0.,-1.95495,0.));
#6228=CARTESIAN_POINT('',(-0.24505,-0.995,-3.00099698131059E-17));
#6229=CARTESIAN_POINT('Origin',(0.,-1.975,0.));
#6230=CARTESIAN_POINT('',(-0.2,-2.,-2.44929359829471E-17));
#6231=CARTESIAN_POINT('Origin',(0.,-2.,0.));
#6232=CARTESIAN_POINT('',(-0.225,-1.975,-2.75545529808154E-17));
#6233=CARTESIAN_POINT('Origin',(0.,-2.,0.));
#6234=CARTESIAN_POINT('Origin',(0.115470053837925,-0.5,-0.2));
#6235=CARTESIAN_POINT('',(0.23094010767585,-0.5,0.));
#6236=CARTESIAN_POINT('',(0.115470053837925,-0.5,-0.2));
#6237=CARTESIAN_POINT('',(0.23094010767585,-0.5,0.));
#6238=CARTESIAN_POINT('',(0.115470053837925,-0.8,-0.2));
#6239=CARTESIAN_POINT('',(0.115470053837925,-0.5,-0.2));
#6240=CARTESIAN_POINT('',(0.23094010767585,-0.8,0.));
#6241=CARTESIAN_POINT('',(0.23094010767585,-0.8,0.));
#6242=CARTESIAN_POINT('',(0.23094010767585,-0.5,0.));
#6243=CARTESIAN_POINT('Origin',(-0.115470053837925,-0.5,-0.2));
#6244=CARTESIAN_POINT('',(-0.115470053837925,-0.5,-0.2));
#6245=CARTESIAN_POINT('',(0.115470053837925,-0.5,-0.2));
#6246=CARTESIAN_POINT('',(-0.115470053837925,-0.8,-0.2));
#6247=CARTESIAN_POINT('',(-0.115470053837925,-0.5,-0.2));
#6248=CARTESIAN_POINT('',(0.115470053837925,-0.8,-0.2));
#6249=CARTESIAN_POINT('Origin',(-0.23094010767585,-0.5,-2.77555756156289E-17));
#6250=CARTESIAN_POINT('',(-0.23094010767585,-0.5,-2.82820063659975E-17));
#6251=CARTESIAN_POINT('',(-0.115470053837925,-0.5,-0.2));
#6252=CARTESIAN_POINT('',(-0.23094010767585,-0.8,-2.77555756156289E-17));
#6253=CARTESIAN_POINT('',(-0.23094010767585,-0.5,-2.82820063659975E-17));
#6254=CARTESIAN_POINT('',(-0.115470053837925,-0.8,-0.2));
#6255=CARTESIAN_POINT('Origin',(-0.115470053837925,-0.5,0.2));
#6256=CARTESIAN_POINT('',(-0.115470053837925,-0.5,0.2));
#6257=CARTESIAN_POINT('',(-0.23094010767585,-0.5,-2.82820063659975E-17));
#6258=CARTESIAN_POINT('',(-0.115470053837925,-0.8,0.2));
#6259=CARTESIAN_POINT('',(-0.115470053837925,-0.5,0.2));
#6260=CARTESIAN_POINT('',(-0.23094010767585,-0.8,-2.82820063659975E-17));
#6261=CARTESIAN_POINT('Origin',(0.115470053837925,-0.5,0.2));
#6262=CARTESIAN_POINT('',(0.115470053837925,-0.5,0.2));
#6263=CARTESIAN_POINT('',(-0.115470053837925,-0.5,0.2));
#6264=CARTESIAN_POINT('',(0.115470053837925,-0.8,0.2));
#6265=CARTESIAN_POINT('',(0.115470053837925,-0.5,0.2));
#6266=CARTESIAN_POINT('',(-0.115470053837925,-0.8,0.2));
#6267=CARTESIAN_POINT('Origin',(0.23094010767585,-0.5,0.));
#6268=CARTESIAN_POINT('',(0.115470053837925,-0.5,0.2));
#6269=CARTESIAN_POINT('',(0.115470053837925,-0.8,0.2));
#6270=CARTESIAN_POINT('Origin',(0.,-0.5,0.));
#6271=CARTESIAN_POINT('Origin',(0.,-0.8,0.));
#6272=CARTESIAN_POINT('',(0.,0.,0.));
#6273=CARTESIAN_POINT('',(0.,-4.,3.3));
#6274=CARTESIAN_POINT('',(1.,-4.,1.));
#6275=CARTESIAN_POINT('',(1.,-5.6,1.6));
#6276=CARTESIAN_POINT('',(1.,-2.4,1.6));
#6277=CARTESIAN_POINT('',(1.,-5.2,4.35));
#6278=CARTESIAN_POINT('',(29.,-4.,1.));
#6279=CARTESIAN_POINT('',(29.,-5.6,1.6));
#6280=CARTESIAN_POINT('',(29.,-2.4,1.6));
#6281=CARTESIAN_POINT('',(29.,-5.2,4.35));
#6282=CARTESIAN_POINT('',(0.,4.,3.3));
#6283=CARTESIAN_POINT('',(1.,4.,1.));
#6284=CARTESIAN_POINT('',(1.,2.4,1.6));
#6285=CARTESIAN_POINT('',(1.,5.6,1.6));
#6286=CARTESIAN_POINT('',(1.,2.8,4.35));
#6287=CARTESIAN_POINT('',(29.,4.,1.));
#6288=CARTESIAN_POINT('',(29.,2.4,1.6));
#6289=CARTESIAN_POINT('',(29.,5.6,1.6));
#6290=CARTESIAN_POINT('',(29.,2.8,4.35));
#6291=CARTESIAN_POINT('',(0.,0.,0.));
#6292=CARTESIAN_POINT('',(3.5,-5.5,2.));
#6293=CARTESIAN_POINT('',(3.5,5.5,2.));
#6294=CARTESIAN_POINT('',(23.,0.,0.));
#6295=CARTESIAN_POINT('',(26.5,-5.5,2.));
#6296=CARTESIAN_POINT('',(26.5,5.5,2.));
#6297=CARTESIAN_POINT('',(0.,0.,0.));
#6298=CARTESIAN_POINT('',(21.8,0.,0.));
#6299=CARTESIAN_POINT('',(0.,0.,0.));
#6300=CARTESIAN_POINT('Origin',(15.,0.,6.6));
#6301=CARTESIAN_POINT('',(14.67,-4.04133443718627E-17,8.2));
#6302=CARTESIAN_POINT('Origin',(15.,0.,8.2));
#6303=CARTESIAN_POINT('',(14.67,-4.04133443718627E-17,6.6));
#6304=CARTESIAN_POINT('',(14.67,-4.04133443718627E-17,6.6));
#6305=CARTESIAN_POINT('Origin',(15.,0.,6.6));
#6306=CARTESIAN_POINT('Origin',(15.,0.,6.6));
#6307=CARTESIAN_POINT('',(13.5,-1.83697019872103E-16,8.2));
#6308=CARTESIAN_POINT('Origin',(15.,0.,8.2));
#6309=CARTESIAN_POINT('',(13.5,-1.83697019872103E-16,6.6));
#6310=CARTESIAN_POINT('',(13.5,-1.83697019872103E-16,6.6));
#6311=CARTESIAN_POINT('Origin',(15.,0.,6.6));
#6312=CARTESIAN_POINT('Origin',(15.,0.,8.2));
#6313=CARTESIAN_POINT('Origin',(15.,0.,6.6));
#6314=CARTESIAN_POINT('',(0.,0.,0.));
#6315=CARTESIAN_POINT('Origin',(0.,0.,0.));
#6316=CARTESIAN_POINT('',(-0.32,0.16,3.91886975727153E-17));
#6317=CARTESIAN_POINT('Origin',(0.,0.16,0.));
#6318=CARTESIAN_POINT('',(-0.32,0.,3.91886975727153E-17));
#6319=CARTESIAN_POINT('',(-0.32,0.,3.91886975727153E-17));
#6320=CARTESIAN_POINT('Origin',(0.,0.,0.));
#6321=CARTESIAN_POINT('Origin',(0.,0.,0.));
#6322=CARTESIAN_POINT('',(-0.6,0.16,7.34788079488412E-17));
#6323=CARTESIAN_POINT('Origin',(0.,0.16,0.));
#6324=CARTESIAN_POINT('',(-0.6,0.,7.34788079488412E-17));
#6325=CARTESIAN_POINT('',(-0.6,0.,7.34788079488412E-17));
#6326=CARTESIAN_POINT('Origin',(0.,0.,0.));
#6327=CARTESIAN_POINT('Origin',(0.,0.16,0.));
#6328=CARTESIAN_POINT('Origin',(0.,0.,0.));
#6329=CARTESIAN_POINT('',(0.,0.,0.));
#6330=CARTESIAN_POINT('Origin',(0.45,0.6,0.));
#6331=CARTESIAN_POINT('',(-0.45,0.6,-5.51091059616309E-17));
#6332=CARTESIAN_POINT('Origin',(0.,0.6,0.));
#6333=CARTESIAN_POINT('Origin',(0.,0.575,0.));
#6334=CARTESIAN_POINT('',(-0.5,0.55,-6.12323399573677E-17));
#6335=CARTESIAN_POINT('Origin',(0.,0.55,0.));
#6336=CARTESIAN_POINT('',(-0.475,0.575,-5.81707229594993E-17));
#6337=CARTESIAN_POINT('Origin',(0.,0.29,0.));
#6338=CARTESIAN_POINT('',(-0.5,0.0299999999999998,-6.12323399573677E-17));
#6339=CARTESIAN_POINT('Origin',(0.,0.0299999999999998,0.));
#6340=CARTESIAN_POINT('',(-0.5,0.29,-6.12323399573677E-17));
#6341=CARTESIAN_POINT('Origin',(0.,0.0150000000000001,0.));
#6342=CARTESIAN_POINT('',(-0.47,7.11236625150491E-17,-5.75583995599256E-17));
#6343=CARTESIAN_POINT('Origin',(0.,0.,0.));
#6344=CARTESIAN_POINT('',(-0.485,0.0150000000000001,-5.93953697586466E-17));
#6345=CARTESIAN_POINT('Origin',(0.32,0.,0.));
#6346=CARTESIAN_POINT('',(-0.32,-6.93889390390723E-18,-3.91886975727153E-17));
#6347=CARTESIAN_POINT('Origin',(0.,0.,0.));
#6348=CARTESIAN_POINT('Origin',(0.,-0.02,0.));
#6349=CARTESIAN_POINT('',(-0.2942,-0.0515999999999999,3.60291088309151E-17));
#6350=CARTESIAN_POINT('Origin',(0.,-0.0515999999999999,0.));
#6351=CARTESIAN_POINT('',(-0.31,-0.02,-3.7964050773568E-17));
#6352=CARTESIAN_POINT('Origin',(0.,-1.24,0.));
#6353=CARTESIAN_POINT('',(-0.2942,-2.4458,3.60291088309151E-17));
#6354=CARTESIAN_POINT('Origin',(0.,-2.4458,0.));
#6355=CARTESIAN_POINT('',(-0.2942,-1.24,-3.60291088309151E-17));
#6356=CARTESIAN_POINT('Origin',(0.,-2.47,0.));
#6357=CARTESIAN_POINT('',(-0.24,-2.5,-2.93915231795365E-17));
#6358=CARTESIAN_POINT('Origin',(0.,-2.5,0.));
#6359=CARTESIAN_POINT('',(-0.27,-2.47,-3.30654635769785E-17));
#6360=CARTESIAN_POINT('Origin',(0.,-2.5,0.));
#6361=CARTESIAN_POINT('Origin',(0.144337567297406,-0.6,-0.25));
#6362=CARTESIAN_POINT('',(0.288675134594813,-0.6,0.));
#6363=CARTESIAN_POINT('',(0.144337567297406,-0.6,-0.25));
#6364=CARTESIAN_POINT('',(0.288675134594813,-0.6,0.));
#6365=CARTESIAN_POINT('',(0.144337567297406,-0.96,-0.25));
#6366=CARTESIAN_POINT('',(0.144337567297406,-0.6,-0.25));
#6367=CARTESIAN_POINT('',(0.288675134594813,-0.96,0.));
#6368=CARTESIAN_POINT('',(0.288675134594813,-0.96,0.));
#6369=CARTESIAN_POINT('',(0.288675134594813,-0.6,0.));
#6370=CARTESIAN_POINT('Origin',(-0.144337567297406,-0.6,-0.25));
#6371=CARTESIAN_POINT('',(-0.144337567297406,-0.6,-0.25));
#6372=CARTESIAN_POINT('',(0.144337567297406,-0.6,-0.25));
#6373=CARTESIAN_POINT('',(-0.144337567297406,-0.96,-0.25));
#6374=CARTESIAN_POINT('',(-0.144337567297406,-0.6,-0.25));
#6375=CARTESIAN_POINT('',(0.144337567297406,-0.96,-0.25));
#6376=CARTESIAN_POINT('Origin',(-0.288675134594813,-0.6,-8.32667268468867E-17));
#6377=CARTESIAN_POINT('',(-0.288675134594813,-0.6,-3.53525079574969E-17));
#6378=CARTESIAN_POINT('',(-0.144337567297406,-0.6,-0.25));
#6379=CARTESIAN_POINT('',(-0.288675134594813,-0.96,-5.55111512312578E-17));
#6380=CARTESIAN_POINT('',(-0.288675134594813,-0.6,-3.53525079574969E-17));
#6381=CARTESIAN_POINT('',(-0.144337567297406,-0.96,-0.25));
#6382=CARTESIAN_POINT('Origin',(-0.144337567297407,-0.6,0.25));
#6383=CARTESIAN_POINT('',(-0.144337567297407,-0.6,0.25));
#6384=CARTESIAN_POINT('',(-0.288675134594813,-0.6,-3.53525079574969E-17));
#6385=CARTESIAN_POINT('',(-0.144337567297407,-0.96,0.25));
#6386=CARTESIAN_POINT('',(-0.144337567297407,-0.6,0.25));
#6387=CARTESIAN_POINT('',(-0.288675134594813,-0.96,-3.53525079574969E-17));
#6388=CARTESIAN_POINT('Origin',(0.144337567297406,-0.6,0.25));
#6389=CARTESIAN_POINT('',(0.144337567297406,-0.6,0.25));
#6390=CARTESIAN_POINT('',(-0.144337567297407,-0.6,0.25));
#6391=CARTESIAN_POINT('',(0.144337567297406,-0.96,0.25));
#6392=CARTESIAN_POINT('',(0.144337567297406,-0.6,0.25));
#6393=CARTESIAN_POINT('',(-0.144337567297407,-0.96,0.25));
#6394=CARTESIAN_POINT('Origin',(0.288675134594813,-0.6,0.));
#6395=CARTESIAN_POINT('',(0.144337567297406,-0.6,0.25));
#6396=CARTESIAN_POINT('',(0.144337567297406,-0.96,0.25));
#6397=CARTESIAN_POINT('Origin',(0.,-0.6,0.));
#6398=CARTESIAN_POINT('Origin',(0.,-0.96,0.));
#6399=CARTESIAN_POINT('',(0.,0.,0.));
#6400=CARTESIAN_POINT('',(0.,0.,0.));
#6401=CARTESIAN_POINT('',(15.,-4.,3.3));
#6402=CARTESIAN_POINT('',(15.,4.,3.3));
#6403=CARTESIAN_POINT('',(3.,0.,0.));
#6404=CARTESIAN_POINT('',(6.5,0.,0.));
#6405=CARTESIAN_POINT('',(13.,-5.5,3.));
#6406=CARTESIAN_POINT('',(13.,-5.5,5.));
#6407=CARTESIAN_POINT('',(13.,5.5,3.));
#6408=CARTESIAN_POINT('',(13.,5.5,5.));
#6409=CARTESIAN_POINT('',(17.,-5.5,3.));
#6410=CARTESIAN_POINT('',(17.,-5.5,5.));
#6411=CARTESIAN_POINT('',(17.,5.5,3.));
#6412=CARTESIAN_POINT('',(17.,5.5,5.));
#6413=CARTESIAN_POINT('',(14.,-2.2,6.6));
#6414=CARTESIAN_POINT('',(14.,2.2,6.6));
#6415=CARTESIAN_POINT('',(16.,-2.2,6.6));
#6416=CARTESIAN_POINT('',(16.,2.2,6.6));
#6417=CARTESIAN_POINT('',(0.,0.,0.));
#6418=CARTESIAN_POINT('',(15.,0.,8.2));
#6419=CARTESIAN_POINT('',(15.,0.,8.36));
#6420=CARTESIAN_POINT('',(0.,0.,0.));
#6421=CARTESIAN_POINT('',(0.,0.,0.));
#6422=UNCERTAINTY_MEASURE_WITH_UNIT(LENGTH_MEASURE(0.001),#6464,
'DISTANCE_ACCURACY_VALUE',
'Maximum model space distance between geometric entities at asserted c
onnectivities');
#6423=UNCERTAINTY_MEASURE_WITH_UNIT(LENGTH_MEASURE(0.001),#6464,
'DISTANCE_ACCURACY_VALUE',
'Maximum model space distance between geometric entities at asserted c
onnectivities');
#6424=UNCERTAINTY_MEASURE_WITH_UNIT(LENGTH_MEASURE(0.001),#6464,
'DISTANCE_ACCURACY_VALUE',
'Maximum model space distance between geometric entities at asserted c
onnectivities');
#6425=UNCERTAINTY_MEASURE_WITH_UNIT(LENGTH_MEASURE(0.001),#6464,
'DISTANCE_ACCURACY_VALUE',
'Maximum model space distance between geometric entities at asserted c
onnectivities');
#6426=UNCERTAINTY_MEASURE_WITH_UNIT(LENGTH_MEASURE(0.001),#6464,
'DISTANCE_ACCURACY_VALUE',
'Maximum model space distance between geometric entities at asserted c
onnectivities');
#6427=UNCERTAINTY_MEASURE_WITH_UNIT(LENGTH_MEASURE(0.001),#6464,
'DISTANCE_ACCURACY_VALUE',
'Maximum model space distance between geometric entities at asserted c
onnectivities');
#6428=UNCERTAINTY_MEASURE_WITH_UNIT(LENGTH_MEASURE(0.001),#6464,
'DISTANCE_ACCURACY_VALUE',
'Maximum model space distance between geometric entities at asserted c
onnectivities');
#6429=UNCERTAINTY_MEASURE_WITH_UNIT(LENGTH_MEASURE(0.001),#6464,
'DISTANCE_ACCURACY_VALUE',
'Maximum model space distance between geometric entities at asserted c
onnectivities');
#6430=UNCERTAINTY_MEASURE_WITH_UNIT(LENGTH_MEASURE(0.001),#6464,
'DISTANCE_ACCURACY_VALUE',
'Maximum model space distance between geometric entities at asserted c
onnectivities');
#6431=UNCERTAINTY_MEASURE_WITH_UNIT(LENGTH_MEASURE(0.001),#6464,
'DISTANCE_ACCURACY_VALUE',
'Maximum model space distance between geometric entities at asserted c
onnectivities');
#6432=UNCERTAINTY_MEASURE_WITH_UNIT(LENGTH_MEASURE(0.001),#6464,
'DISTANCE_ACCURACY_VALUE',
'Maximum model space distance between geometric entities at asserted c
onnectivities');
#6433=UNCERTAINTY_MEASURE_WITH_UNIT(LENGTH_MEASURE(0.001),#6464,
'DISTANCE_ACCURACY_VALUE',
'Maximum model space distance between geometric entities at asserted c
onnectivities');
#6434=UNCERTAINTY_MEASURE_WITH_UNIT(LENGTH_MEASURE(0.001),#6464,
'DISTANCE_ACCURACY_VALUE',
'Maximum model space distance between geometric entities at asserted c
onnectivities');
#6435=UNCERTAINTY_MEASURE_WITH_UNIT(LENGTH_MEASURE(0.001),#6464,
'DISTANCE_ACCURACY_VALUE',
'Maximum model space distance between geometric entities at asserted c
onnectivities');
#6436=UNCERTAINTY_MEASURE_WITH_UNIT(LENGTH_MEASURE(0.001),#6464,
'DISTANCE_ACCURACY_VALUE',
'Maximum model space distance between geometric entities at asserted c
onnectivities');
#6437=UNCERTAINTY_MEASURE_WITH_UNIT(LENGTH_MEASURE(0.001),#6464,
'DISTANCE_ACCURACY_VALUE',
'Maximum model space distance between geometric entities at asserted c
onnectivities');
#6438=UNCERTAINTY_MEASURE_WITH_UNIT(LENGTH_MEASURE(0.001),#6464,
'DISTANCE_ACCURACY_VALUE',
'Maximum model space distance between geometric entities at asserted c
onnectivities');
#6439=UNCERTAINTY_MEASURE_WITH_UNIT(LENGTH_MEASURE(0.001),#6464,
'DISTANCE_ACCURACY_VALUE',
'Maximum model space distance between geometric entities at asserted c
onnectivities');
#6440=UNCERTAINTY_MEASURE_WITH_UNIT(LENGTH_MEASURE(0.001),#6464,
'DISTANCE_ACCURACY_VALUE',
'Maximum model space distance between geometric entities at asserted c
onnectivities');
#6441=UNCERTAINTY_MEASURE_WITH_UNIT(LENGTH_MEASURE(0.001),#6464,
'DISTANCE_ACCURACY_VALUE',
'Maximum model space distance between geometric entities at asserted c
onnectivities');
#6442=UNCERTAINTY_MEASURE_WITH_UNIT(LENGTH_MEASURE(0.001),#6464,
'DISTANCE_ACCURACY_VALUE',
'Maximum model space distance between geometric entities at asserted c
onnectivities');
#6443=(
GEOMETRIC_REPRESENTATION_CONTEXT(3)
GLOBAL_UNCERTAINTY_ASSIGNED_CONTEXT((#6422))
GLOBAL_UNIT_ASSIGNED_CONTEXT((#6464,#6466,#6467))
REPRESENTATION_CONTEXT('','3D')
);
#6444=(
GEOMETRIC_REPRESENTATION_CONTEXT(3)
GLOBAL_UNCERTAINTY_ASSIGNED_CONTEXT((#6423))
GLOBAL_UNIT_ASSIGNED_CONTEXT((#6464,#6466,#6467))
REPRESENTATION_CONTEXT('','3D')
);
#6445=(
GEOMETRIC_REPRESENTATION_CONTEXT(3)
GLOBAL_UNCERTAINTY_ASSIGNED_CONTEXT((#6424))
GLOBAL_UNIT_ASSIGNED_CONTEXT((#6464,#6466,#6467))
REPRESENTATION_CONTEXT('','3D')
);
#6446=(
GEOMETRIC_REPRESENTATION_CONTEXT(3)
GLOBAL_UNCERTAINTY_ASSIGNED_CONTEXT((#6425))
GLOBAL_UNIT_ASSIGNED_CONTEXT((#6464,#6466,#6467))
REPRESENTATION_CONTEXT('','3D')
);
#6447=(
GEOMETRIC_REPRESENTATION_CONTEXT(3)
GLOBAL_UNCERTAINTY_ASSIGNED_CONTEXT((#6426))
GLOBAL_UNIT_ASSIGNED_CONTEXT((#6464,#6466,#6467))
REPRESENTATION_CONTEXT('','3D')
);
#6448=(
GEOMETRIC_REPRESENTATION_CONTEXT(3)
GLOBAL_UNCERTAINTY_ASSIGNED_CONTEXT((#6427))
GLOBAL_UNIT_ASSIGNED_CONTEXT((#6464,#6466,#6467))
REPRESENTATION_CONTEXT('','3D')
);
#6449=(
GEOMETRIC_REPRESENTATION_CONTEXT(3)
GLOBAL_UNCERTAINTY_ASSIGNED_CONTEXT((#6428))
GLOBAL_UNIT_ASSIGNED_CONTEXT((#6464,#6466,#6467))
REPRESENTATION_CONTEXT('','3D')
);
#6450=(
GEOMETRIC_REPRESENTATION_CONTEXT(3)
GLOBAL_UNCERTAINTY_ASSIGNED_CONTEXT((#6429))
GLOBAL_UNIT_ASSIGNED_CONTEXT((#6464,#6466,#6467))
REPRESENTATION_CONTEXT('','3D')
);
#6451=(
GEOMETRIC_REPRESENTATION_CONTEXT(3)
GLOBAL_UNCERTAINTY_ASSIGNED_CONTEXT((#6430))
GLOBAL_UNIT_ASSIGNED_CONTEXT((#6464,#6466,#6467))
REPRESENTATION_CONTEXT('','3D')
);
#6452=(
GEOMETRIC_REPRESENTATION_CONTEXT(3)
GLOBAL_UNCERTAINTY_ASSIGNED_CONTEXT((#6431))
GLOBAL_UNIT_ASSIGNED_CONTEXT((#6464,#6466,#6467))
REPRESENTATION_CONTEXT('','3D')
);
#6453=(
GEOMETRIC_REPRESENTATION_CONTEXT(3)
GLOBAL_UNCERTAINTY_ASSIGNED_CONTEXT((#6432))
GLOBAL_UNIT_ASSIGNED_CONTEXT((#6464,#6466,#6467))
REPRESENTATION_CONTEXT('','3D')
);
#6454=(
GEOMETRIC_REPRESENTATION_CONTEXT(3)
GLOBAL_UNCERTAINTY_ASSIGNED_CONTEXT((#6433))
GLOBAL_UNIT_ASSIGNED_CONTEXT((#6464,#6466,#6467))
REPRESENTATION_CONTEXT('','3D')
);
#6455=(
GEOMETRIC_REPRESENTATION_CONTEXT(3)
GLOBAL_UNCERTAINTY_ASSIGNED_CONTEXT((#6434))
GLOBAL_UNIT_ASSIGNED_CONTEXT((#6464,#6466,#6467))
REPRESENTATION_CONTEXT('','3D')
);
#6456=(
GEOMETRIC_REPRESENTATION_CONTEXT(3)
GLOBAL_UNCERTAINTY_ASSIGNED_CONTEXT((#6435))
GLOBAL_UNIT_ASSIGNED_CONTEXT((#6464,#6466,#6467))
REPRESENTATION_CONTEXT('','3D')
);
#6457=(
GEOMETRIC_REPRESENTATION_CONTEXT(3)
GLOBAL_UNCERTAINTY_ASSIGNED_CONTEXT((#6436))
GLOBAL_UNIT_ASSIGNED_CONTEXT((#6464,#6466,#6467))
REPRESENTATION_CONTEXT('','3D')
);
#6458=(
GEOMETRIC_REPRESENTATION_CONTEXT(3)
GLOBAL_UNCERTAINTY_ASSIGNED_CONTEXT((#6437))
GLOBAL_UNIT_ASSIGNED_CONTEXT((#6464,#6466,#6467))
REPRESENTATION_CONTEXT('','3D')
);
#6459=(
GEOMETRIC_REPRESENTATION_CONTEXT(3)
GLOBAL_UNCERTAINTY_ASSIGNED_CONTEXT((#6438))
GLOBAL_UNIT_ASSIGNED_CONTEXT((#6464,#6466,#6467))
REPRESENTATION_CONTEXT('','3D')
);
#6460=(
GEOMETRIC_REPRESENTATION_CONTEXT(3)
GLOBAL_UNCERTAINTY_ASSIGNED_CONTEXT((#6439))
GLOBAL_UNIT_ASSIGNED_CONTEXT((#6464,#6466,#6467))
REPRESENTATION_CONTEXT('','3D')
);
#6461=(
GEOMETRIC_REPRESENTATION_CONTEXT(3)
GLOBAL_UNCERTAINTY_ASSIGNED_CONTEXT((#6440))
GLOBAL_UNIT_ASSIGNED_CONTEXT((#6464,#6466,#6467))
REPRESENTATION_CONTEXT('','3D')
);
#6462=(
GEOMETRIC_REPRESENTATION_CONTEXT(3)
GLOBAL_UNCERTAINTY_ASSIGNED_CONTEXT((#6441))
GLOBAL_UNIT_ASSIGNED_CONTEXT((#6464,#6466,#6467))
REPRESENTATION_CONTEXT('','3D')
);
#6463=(
GEOMETRIC_REPRESENTATION_CONTEXT(3)
GLOBAL_UNCERTAINTY_ASSIGNED_CONTEXT((#6442))
GLOBAL_UNIT_ASSIGNED_CONTEXT((#6464,#6466,#6467))
REPRESENTATION_CONTEXT('','3D')
);
#6464=(
LENGTH_UNIT()
NAMED_UNIT(*)
SI_UNIT(.CENTI.,.METRE.)
);
#6465=(
LENGTH_UNIT()
NAMED_UNIT(*)
SI_UNIT($,.METRE.)
);
#6466=(
NAMED_UNIT(*)
PLANE_ANGLE_UNIT()
SI_UNIT($,.RADIAN.)
);
#6467=(
NAMED_UNIT(*)
SI_UNIT($,.STERADIAN.)
SOLID_ANGLE_UNIT()
);
#6468=SHAPE_DEFINITION_REPRESENTATION(#6488,#6560);
#6469=SHAPE_DEFINITION_REPRESENTATION(#6489,#6561);
#6470=SHAPE_DEFINITION_REPRESENTATION(#6490,#6562);
#6471=SHAPE_DEFINITION_REPRESENTATION(#6491,#6563);
#6472=SHAPE_DEFINITION_REPRESENTATION(#6492,#6564);
#6473=SHAPE_DEFINITION_REPRESENTATION(#6493,#6565);
#6474=SHAPE_DEFINITION_REPRESENTATION(#6494,#6566);
#6475=SHAPE_DEFINITION_REPRESENTATION(#6495,#6567);
#6476=SHAPE_DEFINITION_REPRESENTATION(#6496,#6568);
#6477=SHAPE_DEFINITION_REPRESENTATION(#6497,#6569);
#6478=SHAPE_DEFINITION_REPRESENTATION(#6498,#6570);
#6479=SHAPE_DEFINITION_REPRESENTATION(#6499,#6571);
#6480=SHAPE_DEFINITION_REPRESENTATION(#6500,#6572);
#6481=SHAPE_DEFINITION_REPRESENTATION(#6501,#6573);
#6482=SHAPE_DEFINITION_REPRESENTATION(#6504,#6574);
#6483=SHAPE_DEFINITION_REPRESENTATION(#6505,#6575);
#6484=SHAPE_DEFINITION_REPRESENTATION(#6506,#6576);
#6485=SHAPE_DEFINITION_REPRESENTATION(#6534,#6577);
#6486=SHAPE_DEFINITION_REPRESENTATION(#6535,#6578);
#6487=SHAPE_DEFINITION_REPRESENTATION(#6536,#6579);
#6488=PRODUCT_DEFINITION_SHAPE('',$,#6581);
#6489=PRODUCT_DEFINITION_SHAPE('',$,#6582);
#6490=PRODUCT_DEFINITION_SHAPE('',$,#6583);
#6491=PRODUCT_DEFINITION_SHAPE('',$,#6584);
#6492=PRODUCT_DEFINITION_SHAPE('',$,#6585);
#6493=PRODUCT_DEFINITION_SHAPE('',$,#6586);
#6494=PRODUCT_DEFINITION_SHAPE('',$,#6587);
#6495=PRODUCT_DEFINITION_SHAPE('',$,#6588);
#6496=PRODUCT_DEFINITION_SHAPE('',$,#6589);
#6497=PRODUCT_DEFINITION_SHAPE('',$,#6590);
#6498=PRODUCT_DEFINITION_SHAPE('',$,#6591);
#6499=PRODUCT_DEFINITION_SHAPE('',$,#6592);
#6500=PRODUCT_DEFINITION_SHAPE('',$,#6593);
#6501=PRODUCT_DEFINITION_SHAPE('',$,#6594);
#6502=PRODUCT_DEFINITION_SHAPE($,$,#167);
#6503=PRODUCT_DEFINITION_SHAPE($,$,#168);
#6504=PRODUCT_DEFINITION_SHAPE('',$,#6595);
#6505=PRODUCT_DEFINITION_SHAPE('',$,#6596);
#6506=PRODUCT_DEFINITION_SHAPE('',$,#6597);
#6507=PRODUCT_DEFINITION_SHAPE($,$,#169);
#6508=PRODUCT_DEFINITION_SHAPE($,$,#170);
#6509=PRODUCT_DEFINITION_SHAPE($,$,#171);
#6510=PRODUCT_DEFINITION_SHAPE($,$,#172);
#6511=PRODUCT_DEFINITION_SHAPE($,$,#173);
#6512=PRODUCT_DEFINITION_SHAPE($,$,#174);
#6513=PRODUCT_DEFINITION_SHAPE($,$,#175);
#6514=PRODUCT_DEFINITION_SHAPE($,$,#176);
#6515=PRODUCT_DEFINITION_SHAPE($,$,#177);
#6516=PRODUCT_DEFINITION_SHAPE($,$,#178);
#6517=PRODUCT_DEFINITION_SHAPE($,$,#179);
#6518=PRODUCT_DEFINITION_SHAPE($,$,#180);
#6519=PRODUCT_DEFINITION_SHAPE($,$,#181);
#6520=PRODUCT_DEFINITION_SHAPE($,$,#182);
#6521=PRODUCT_DEFINITION_SHAPE($,$,#183);
#6522=PRODUCT_DEFINITION_SHAPE($,$,#184);
#6523=PRODUCT_DEFINITION_SHAPE($,$,#185);
#6524=PRODUCT_DEFINITION_SHAPE($,$,#186);
#6525=PRODUCT_DEFINITION_SHAPE($,$,#187);
#6526=PRODUCT_DEFINITION_SHAPE($,$,#188);
#6527=PRODUCT_DEFINITION_SHAPE($,$,#189);
#6528=PRODUCT_DEFINITION_SHAPE($,$,#190);
#6529=PRODUCT_DEFINITION_SHAPE($,$,#191);
#6530=PRODUCT_DEFINITION_SHAPE($,$,#192);
#6531=PRODUCT_DEFINITION_SHAPE($,$,#193);
#6532=PRODUCT_DEFINITION_SHAPE($,$,#194);
#6533=PRODUCT_DEFINITION_SHAPE($,$,#195);
#6534=PRODUCT_DEFINITION_SHAPE('',$,#6598);
#6535=PRODUCT_DEFINITION_SHAPE('',$,#6599);
#6536=PRODUCT_DEFINITION_SHAPE('',$,#6600);
#6537=PRODUCT_DEFINITION_SHAPE($,$,#196);
#6538=PRODUCT_DEFINITION_SHAPE($,$,#197);
#6539=PRODUCT_DEFINITION_SHAPE($,$,#198);
#6540=PRODUCT_DEFINITION_SHAPE($,$,#199);
#6541=PRODUCT_DEFINITION_SHAPE($,$,#200);
#6542=PRODUCT_DEFINITION_SHAPE($,$,#201);
#6543=PRODUCT_DEFINITION_SHAPE($,$,#202);
#6544=PRODUCT_DEFINITION_SHAPE($,$,#203);
#6545=PRODUCT_DEFINITION_SHAPE($,$,#204);
#6546=PRODUCT_DEFINITION_SHAPE($,$,#205);
#6547=PRODUCT_DEFINITION_SHAPE($,$,#206);
#6548=PRODUCT_DEFINITION_SHAPE($,$,#207);
#6549=PRODUCT_DEFINITION_SHAPE($,$,#208);
#6550=PRODUCT_DEFINITION_SHAPE($,$,#209);
#6551=PRODUCT_DEFINITION_SHAPE($,$,#210);
#6552=PRODUCT_DEFINITION_SHAPE($,$,#211);
#6553=PRODUCT_DEFINITION_SHAPE($,$,#212);
#6554=PRODUCT_DEFINITION_SHAPE($,$,#213);
#6555=PRODUCT_DEFINITION_SHAPE($,$,#214);
#6556=PRODUCT_DEFINITION_SHAPE($,$,#215);
#6557=PRODUCT_DEFINITION_SHAPE($,$,#216);
#6558=PRODUCT_DEFINITION_SHAPE($,$,#217);
#6559=PRODUCT_DEFINITION_SHAPE($,$,#218);
#6560=SHAPE_REPRESENTATION('',(#3835,#4265,#4266),#6443);
#6561=SHAPE_REPRESENTATION('',(#3836,#4173,#4174,#4175,#4176,#4177,#4178,
#4179,#4180,#4181,#4182,#4183,#4184,#4185,#4186,#4187,#4188,#4189,#4190,
#4191,#4192,#4193,#4194,#4195,#4196,#4197,#4198,#4199),#6444);
#6562=SHAPE_REPRESENTATION('',(#3837),#6445);
#6563=SHAPE_REPRESENTATION('',(#3880),#6446);
#6564=SHAPE_REPRESENTATION('',(#3890),#6447);
#6565=SHAPE_REPRESENTATION('',(#3928),#6448);
#6566=SHAPE_REPRESENTATION('',(#3952),#6449);
#6567=SHAPE_REPRESENTATION('',(#3973),#6450);
#6568=SHAPE_REPRESENTATION('',(#3980,#4244,#4245,#4246,#4247,#4248,#4249,
#4250,#4251,#4252,#4253,#4254,#4255,#4256,#4257,#4258,#4259,#4260,#4261,
#4262,#4263,#4264),#6451);
#6569=SHAPE_REPRESENTATION('',(#3981),#6452);
#6570=SHAPE_REPRESENTATION('',(#4022),#6453);
#6571=SHAPE_REPRESENTATION('',(#4044,#4094,#4095),#6454);
#6572=SHAPE_REPRESENTATION('',(#4045),#6455);
#6573=SHAPE_REPRESENTATION('',(#4077),#6456);
#6574=SHAPE_REPRESENTATION('',(#4096),#6457);
#6575=SHAPE_REPRESENTATION('',(#4121),#6458);
#6576=SHAPE_REPRESENTATION('',(#4147),#6459);
#6577=SHAPE_REPRESENTATION('',(#4200),#6460);
#6578=SHAPE_REPRESENTATION('',(#4209),#6461);
#6579=SHAPE_REPRESENTATION('',(#4218),#6462);
#6580=PRODUCT_DEFINITION_CONTEXT('part definition',#6642,'design');
#6581=PRODUCT_DEFINITION('PAT-110','PAT-110',#6601,#6580);
#6582=PRODUCT_DEFINITION('Shafts supports and end stops',
'Shafts supports and end stops',#6602,#6580);
#6583=PRODUCT_DEFINITION('Base plate','Base plate',#6603,#6580);
#6584=PRODUCT_DEFINITION(
'Precision Shaft - 12 mm Diameter, 300 mm Long',
'Precision Shaft - 12 mm Diameter, 300 mm Long',#6604,#6580);
#6585=PRODUCT_DEFINITION('Relieved shaft support',
'Relieved shaft support',#6605,#6580);
#6586=PRODUCT_DEFINITION('M5x14 Cap Screw','M5x14 Cap Screw',#6606,#6580);
#6587=PRODUCT_DEFINITION('End stop','End stop',#6607,#6580);
#6588=PRODUCT_DEFINITION('Bonded stop pad','Bonded stop pad',#6608,#6580);
#6589=PRODUCT_DEFINITION('Two-bushing carriage','Two-bushing carriage',
#6609,#6580);
#6590=PRODUCT_DEFINITION('Two-bushing housing','Two-bushing housing',#6610,
#6580);
#6591=PRODUCT_DEFINITION('Carriage table','Carriage table',#6611,#6580);
#6592=PRODUCT_DEFINITION('Linear Ball Bushing - 12 x 21 x 30 mm',
'Linear Ball Bushing - 12 x 21 x 30 mm',#6612,#6580);
#6593=PRODUCT_DEFINITION('Steel sleeve','Steel sleeve',#6613,#6580);
#6594=PRODUCT_DEFINITION('Ball retainer (plastic)',
'Ball retainer (plastic)',#6614,#6580);
#6595=PRODUCT_DEFINITION('End retainer','End retainer',#6615,#6580);
#6596=PRODUCT_DEFINITION('Cap Screw - M4x16','Cap Screw - M4x16',#6616,
#6580);
#6597=PRODUCT_DEFINITION('Cap Screw - M5x20','Cap Screw - M5x20',#6617,
#6580);
#6598=PRODUCT_DEFINITION('Grip','Grip',#6618,#6580);
#6599=PRODUCT_DEFINITION('Flat Washer - M6','Flat Washer - M6',#6619,#6580);
#6600=PRODUCT_DEFINITION('Cap Screw - M6x25','Cap Screw - M6x25',#6620,
#6580);
#6601=PRODUCT_DEFINITION_FORMATION('',$,#6644);
#6602=PRODUCT_DEFINITION_FORMATION('',$,#6645);
#6603=PRODUCT_DEFINITION_FORMATION('',$,#6646);
#6604=PRODUCT_DEFINITION_FORMATION('',$,#6647);
#6605=PRODUCT_DEFINITION_FORMATION('',$,#6648);
#6606=PRODUCT_DEFINITION_FORMATION('',$,#6649);
#6607=PRODUCT_DEFINITION_FORMATION('',$,#6650);
#6608=PRODUCT_DEFINITION_FORMATION('',$,#6651);
#6609=PRODUCT_DEFINITION_FORMATION('',$,#6652);
#6610=PRODUCT_DEFINITION_FORMATION('',$,#6653);
#6611=PRODUCT_DEFINITION_FORMATION('',$,#6654);
#6612=PRODUCT_DEFINITION_FORMATION('',$,#6655);
#6613=PRODUCT_DEFINITION_FORMATION('',$,#6656);
#6614=PRODUCT_DEFINITION_FORMATION('',$,#6657);
#6615=PRODUCT_DEFINITION_FORMATION('',$,#6658);
#6616=PRODUCT_DEFINITION_FORMATION('',$,#6659);
#6617=PRODUCT_DEFINITION_FORMATION('',$,#6660);
#6618=PRODUCT_DEFINITION_FORMATION('',$,#6661);
#6619=PRODUCT_DEFINITION_FORMATION('',$,#6662);
#6620=PRODUCT_DEFINITION_FORMATION('',$,#6663);
#6621=PRODUCT_RELATED_PRODUCT_CATEGORY('PAT-110','PAT-110',(#6644));
#6622=PRODUCT_RELATED_PRODUCT_CATEGORY('Shafts supports and end stops',
'Shafts supports and end stops',(#6645));
#6623=PRODUCT_RELATED_PRODUCT_CATEGORY('Base plate','Base plate',(#6646));
#6624=PRODUCT_RELATED_PRODUCT_CATEGORY(
'Precision Shaft - 12 mm Diameter, 300 mm Long',
'Precision Shaft - 12 mm Diameter, 300 mm Long',(#6647));
#6625=PRODUCT_RELATED_PRODUCT_CATEGORY('Relieved shaft support',
'Relieved shaft support',(#6648));
#6626=PRODUCT_RELATED_PRODUCT_CATEGORY('M5x14 Cap Screw',
'M5x14 Cap Screw',(#6649));
#6627=PRODUCT_RELATED_PRODUCT_CATEGORY('End stop','End stop',(#6650));
#6628=PRODUCT_RELATED_PRODUCT_CATEGORY('Bonded stop pad',
'Bonded stop pad',(#6651));
#6629=PRODUCT_RELATED_PRODUCT_CATEGORY('Two-bushing carriage',
'Two-bushing carriage',(#6652));
#6630=PRODUCT_RELATED_PRODUCT_CATEGORY('Two-bushing housing',
'Two-bushing housing',(#6653));
#6631=PRODUCT_RELATED_PRODUCT_CATEGORY('Carriage table',
'Carriage table',(#6654));
#6632=PRODUCT_RELATED_PRODUCT_CATEGORY(
'Linear Ball Bushing - 12 x 21 x 30 mm',
'Linear Ball Bushing - 12 x 21 x 30 mm',(#6655));
#6633=PRODUCT_RELATED_PRODUCT_CATEGORY('Steel sleeve','Steel sleeve',(#6656));
#6634=PRODUCT_RELATED_PRODUCT_CATEGORY('Ball retainer (plastic)',
'Ball retainer (plastic)',(#6657));
#6635=PRODUCT_RELATED_PRODUCT_CATEGORY('End retainer','End retainer',(#6658));
#6636=PRODUCT_RELATED_PRODUCT_CATEGORY('Cap Screw - M4x16',
'Cap Screw - M4x16',(#6659));
#6637=PRODUCT_RELATED_PRODUCT_CATEGORY('Cap Screw - M5x20',
'Cap Screw - M5x20',(#6660));
#6638=PRODUCT_RELATED_PRODUCT_CATEGORY('Grip','Grip',(#6661));
#6639=PRODUCT_RELATED_PRODUCT_CATEGORY('Flat Washer - M6',
'Flat Washer - M6',(#6662));
#6640=PRODUCT_RELATED_PRODUCT_CATEGORY('Cap Screw - M6x25',
'Cap Screw - M6x25',(#6663));
#6641=APPLICATION_PROTOCOL_DEFINITION('international standard',
'automotive_design',2009,#6642);
#6642=APPLICATION_CONTEXT(
'Core Data for Automotive Mechanical Design Process');
#6643=PRODUCT_CONTEXT('part definition',#6642,'mechanical');
#6644=PRODUCT('PAT-110','PAT-110',
'PAT-110',(#6643));
#6645=PRODUCT('Shafts supports and end stops',
'Shafts supports and end stops','Shafts supports and end stops',(#6643));
#6646=PRODUCT('Base plate','Base plate','Base plate',(#6643));
#6647=PRODUCT('Precision Shaft - 12 mm Diameter, 300 mm Long',
'Precision Shaft - 12 mm Diameter, 300 mm Long',
'Precision Shaft - 12 mm Diameter, 300 mm Long',(#6643));
#6648=PRODUCT('Relieved shaft support','Relieved shaft support',
'Relieved shaft support',(#6643));
#6649=PRODUCT('M5x14 Cap Screw','M5x14 Cap Screw','M5x14 Cap Screw',(#6643));
#6650=PRODUCT('End stop','End stop','End stop',(#6643));
#6651=PRODUCT('Bonded stop pad','Bonded stop pad','Bonded stop pad',(#6643));
#6652=PRODUCT('Two-bushing carriage','Two-bushing carriage',
'Two-bushing carriage',(#6643));
#6653=PRODUCT('Two-bushing housing','Two-bushing housing',
'Two-bushing housing',(#6643));
#6654=PRODUCT('Carriage table','Carriage table','Carriage table',(#6643));
#6655=PRODUCT('Linear Ball Bushing - 12 x 21 x 30 mm',
'Linear Ball Bushing - 12 x 21 x 30 mm',
'Linear Ball Bushing - 12 x 21 x 30 mm',(#6643));
#6656=PRODUCT('Steel sleeve','Steel sleeve','Steel sleeve',(#6643));
#6657=PRODUCT('Ball retainer (plastic)','Ball retainer (plastic)',
'Ball retainer (plastic)',(#6643));
#6658=PRODUCT('End retainer','End retainer','End retainer',(#6643));
#6659=PRODUCT('Cap Screw - M4x16','Cap Screw - M4x16',
'Cap Screw - M4x16',(#6643));
#6660=PRODUCT('Cap Screw - M5x20','Cap Screw - M5x20',
'Cap Screw - M5x20',(#6643));
#6661=PRODUCT('Grip','Grip','Grip',(#6643));
#6662=PRODUCT('Flat Washer - M6','Flat Washer - M6','Flat Washer - M6',
(#6643));
#6663=PRODUCT('Cap Screw - M6x25','Cap Screw - M6x25',
'Cap Screw - M6x25',(#6643));
#6664=PRESENTATION_STYLE_ASSIGNMENT((#6671));
#6665=PRESENTATION_STYLE_ASSIGNMENT((#6672));
#6666=PRESENTATION_STYLE_ASSIGNMENT((#6673));
#6667=PRESENTATION_STYLE_ASSIGNMENT((#6674));
#6668=PRESENTATION_STYLE_ASSIGNMENT((#6675));
#6669=PRESENTATION_STYLE_ASSIGNMENT((#6676));
#6670=PRESENTATION_STYLE_ASSIGNMENT((#6677));
#6671=SURFACE_STYLE_USAGE(.BOTH.,#6678);
#6672=SURFACE_STYLE_USAGE(.BOTH.,#6679);
#6673=SURFACE_STYLE_USAGE(.BOTH.,#6680);
#6674=SURFACE_STYLE_USAGE(.BOTH.,#6681);
#6675=SURFACE_STYLE_USAGE(.BOTH.,#6682);
#6676=SURFACE_STYLE_USAGE(.BOTH.,#6683);
#6677=SURFACE_STYLE_USAGE(.BOTH.,#6684);
#6678=SURFACE_SIDE_STYLE('',(#6685));
#6679=SURFACE_SIDE_STYLE('',(#6686));
#6680=SURFACE_SIDE_STYLE('',(#6687));
#6681=SURFACE_SIDE_STYLE('',(#6688));
#6682=SURFACE_SIDE_STYLE('',(#6689));
#6683=SURFACE_SIDE_STYLE('',(#6690));
#6684=SURFACE_SIDE_STYLE('',(#6691));
#6685=SURFACE_STYLE_FILL_AREA(#6692);
#6686=SURFACE_STYLE_FILL_AREA(#6693);
#6687=SURFACE_STYLE_FILL_AREA(#6694);
#6688=SURFACE_STYLE_FILL_AREA(#6695);
#6689=SURFACE_STYLE_FILL_AREA(#6696);
#6690=SURFACE_STYLE_FILL_AREA(#6697);
#6691=SURFACE_STYLE_FILL_AREA(#6698);
#6692=FILL_AREA_STYLE('Steel - Satin',(#6699));
#6693=FILL_AREA_STYLE('CAD Library Painted - Deep blue',(#6700));
#6694=FILL_AREA_STYLE('CAD Library Painted - Steel gray',(#6701));
#6695=FILL_AREA_STYLE('CAD Library Painted - Graphite',(#6702));
#6696=FILL_AREA_STYLE('CAD Library Painted - Engineering blue',(#6703));
#6697=FILL_AREA_STYLE('CAD Library Painted - Off white',(#6704));
#6698=FILL_AREA_STYLE('CAD Library Painted - Light blue',(#6705));
#6699=FILL_AREA_STYLE_COLOUR('Steel - Satin',#6706);
#6700=FILL_AREA_STYLE_COLOUR('CAD Library Painted - Deep blue',#6707);
#6701=FILL_AREA_STYLE_COLOUR('CAD Library Painted - Steel gray',#6708);
#6702=FILL_AREA_STYLE_COLOUR('CAD Library Painted - Graphite',#6709);
#6703=FILL_AREA_STYLE_COLOUR('CAD Library Painted - Engineering blue',#6710);
#6704=FILL_AREA_STYLE_COLOUR('CAD Library Painted - Off white',#6711);
#6705=FILL_AREA_STYLE_COLOUR('CAD Library Painted - Light blue',#6712);
#6706=COLOUR_RGB('Steel - Satin',0.627450980392157,0.627450980392157,0.627450980392157);
#6707=COLOUR_RGB('CAD Library Painted - Deep blue',0.0784313725490196,0.203921568627451,
0.349019607843137);
#6708=COLOUR_RGB('CAD Library Painted - Steel gray',0.592156862745098,0.631372549019608,
0.67843137254902);
#6709=COLOUR_RGB('CAD Library Painted - Graphite',0.0980392156862745,0.109803921568627,
0.125490196078431);
#6710=COLOUR_RGB('CAD Library Painted - Engineering blue',0.12156862745098,
0.356862745098039,0.6);
#6711=COLOUR_RGB('CAD Library Painted - Off white',0.909803921568627,0.901960784313726,
0.858823529411765);
#6712=COLOUR_RGB('CAD Library Painted - Light blue',0.286274509803922,0.552941176470588,
0.780392156862745);
#6713=COLOUR_RGB('Dark Blue',0.08,0.2,0.34);
#6714=FILL_AREA_STYLE_COLOUR('',#6713);
#6715=FILL_AREA_STYLE('',(#6714));
#6716=SURFACE_STYLE_FILL_AREA(#6715);
#6717=SURFACE_SIDE_STYLE('',(#6716));
#6718=SURFACE_STYLE_USAGE(.BOTH.,#6717);
#6719=PRESENTATION_STYLE_ASSIGNMENT((#6718));
#6720=COLOUR_RGB('Light Blue',0.38,0.62,0.78);
#6721=FILL_AREA_STYLE_COLOUR('',#6720);
#6722=FILL_AREA_STYLE('',(#6721));
#6723=SURFACE_STYLE_FILL_AREA(#6722);
#6724=SURFACE_SIDE_STYLE('',(#6723));
#6725=SURFACE_STYLE_USAGE(.BOTH.,#6724);
#6726=PRESENTATION_STYLE_ASSIGNMENT((#6725));
#6727=COLOUR_RGB('Sky Blue',0.24,0.69,0.87);
#6728=FILL_AREA_STYLE_COLOUR('',#6727);
#6729=FILL_AREA_STYLE('',(#6728));
#6730=SURFACE_STYLE_FILL_AREA(#6729);
#6731=SURFACE_SIDE_STYLE('',(#6730));
#6732=SURFACE_STYLE_USAGE(.BOTH.,#6731);
#6733=PRESENTATION_STYLE_ASSIGNMENT((#6732));
#6734=COLOUR_RGB('Grey',0.48,0.52,0.57);
#6735=FILL_AREA_STYLE_COLOUR('',#6734);
#6736=FILL_AREA_STYLE('',(#6735));
#6737=SURFACE_STYLE_FILL_AREA(#6736);
#6738=SURFACE_SIDE_STYLE('',(#6737));
#6739=SURFACE_STYLE_USAGE(.BOTH.,#6738);
#6740=PRESENTATION_STYLE_ASSIGNMENT((#6739));
#6741=COLOUR_RGB('Black',0.12,0.14,0.17);
#6742=FILL_AREA_STYLE_COLOUR('',#6741);
#6743=FILL_AREA_STYLE('',(#6742));
#6744=SURFACE_STYLE_FILL_AREA(#6743);
#6745=SURFACE_SIDE_STYLE('',(#6744));
#6746=SURFACE_STYLE_USAGE(.BOTH.,#6745);
#6747=PRESENTATION_STYLE_ASSIGNMENT((#6746));
#6748=COLOUR_RGB('Off White',0.89,0.88,0.83);
#6749=FILL_AREA_STYLE_COLOUR('',#6748);
#6750=FILL_AREA_STYLE('',(#6749));
#6751=SURFACE_STYLE_FILL_AREA(#6750);
#6752=SURFACE_SIDE_STYLE('',(#6751));
#6753=SURFACE_STYLE_USAGE(.BOTH.,#6752);
#6754=PRESENTATION_STYLE_ASSIGNMENT((#6753));
ENDSEC;
END-ISO-10303-21;
